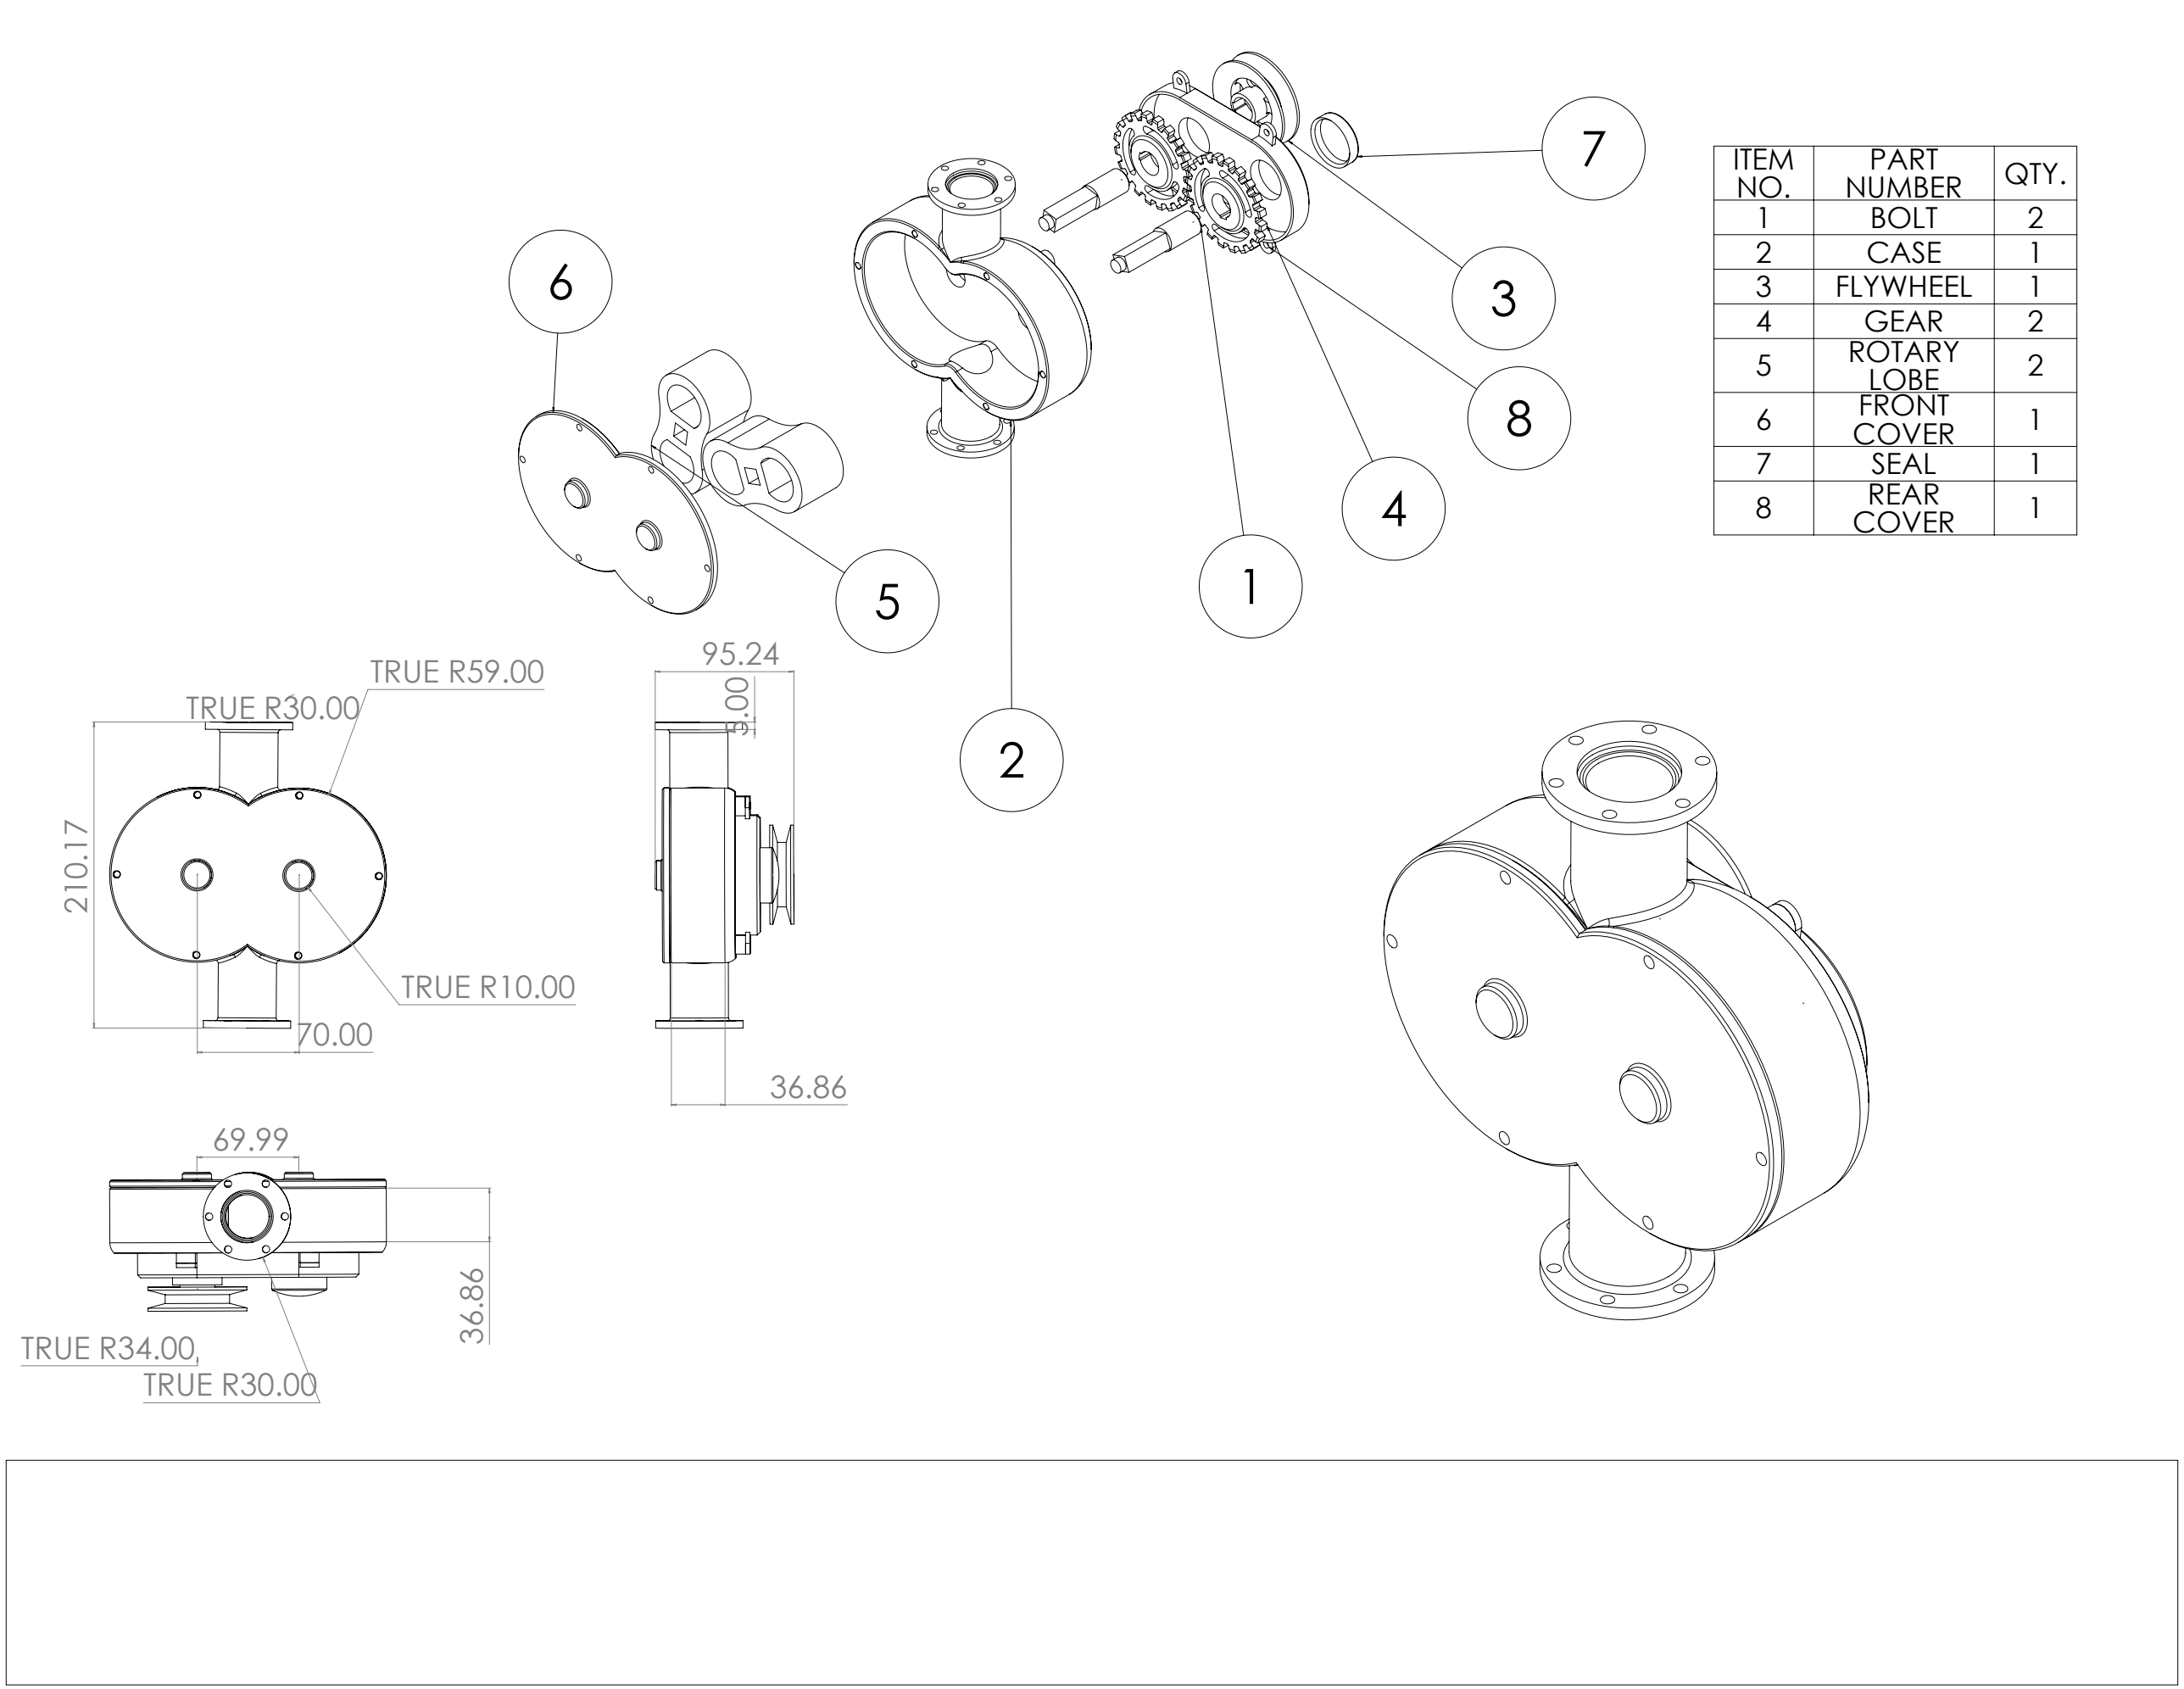
ISO-10303-21;
HEADER;
FILE_DESCRIPTION (('STEP AP214'),
    '1' );
FILE_NAME ('MAS-345',
    '2026-10-24T00:51:42',
    ( '' ),
    ( '' ),
    'SwSTEP 2.0',
    'SolidWorks 2025',
    '' );
FILE_SCHEMA (( 'AUTOMOTIVE_DESIGN' ));
ENDSEC;

DATA;
#1 = DIRECTION ( 'NONE',  ( 1.296372316667914327E-16, 1.000000000000000000, -0.000000000000000000 ) ) ;
#2 = DIRECTION ( 'NONE',  ( -1.000000000000000000, 0.000000000000000000, 0.000000000000000000 ) ) ;
#3 = EDGE_CURVE ( 'NONE', #16867, #19408, #6040, .T. ) ;
#4 = CIRCLE ( 'NONE', #2943, 3.000000000000002665 ) ;
#5 = ORIENTED_EDGE ( 'NONE', *, *, #17834, .T. ) ;
#6 = VECTOR ( 'NONE', #825, 1000.000000000000000 ) ;
#7 = VERTEX_POINT ( 'NONE', #19816 ) ;
#8 = LINE ( 'NONE', #12148, #20561 ) ;
#9 = CARTESIAN_POINT ( 'NONE',  ( 7.505578006075174891, 1.461761173328240959, -55.63523492904085543 ) ) ;
#10 = CYLINDRICAL_SURFACE ( 'NONE', #2581, 1.000000000000000888 ) ;
#11 = DIRECTION ( 'NONE',  ( -0.000000000000000000, 1.000000000000000000, -0.000000000000000000 ) ) ;
#12 = DIRECTION ( 'NONE',  ( -6.505213034913038160E-19, -3.903127820947822896E-18, -1.000000000000000000 ) ) ;
#13 = ORIENTED_EDGE ( 'NONE', *, *, #8232, .T. ) ;
#14 = LINE ( 'NONE', #10421, #6182 ) ;
#15 = CARTESIAN_POINT ( 'NONE',  ( -11.08851315719095609, 40.00000000000000000, -54.00022650832062254 ) ) ;
#16 = VERTEX_POINT ( 'NONE', #2397 ) ;
#17 = DIRECTION ( 'NONE',  ( 0.000000000000000000, -1.000000000000000000, 0.000000000000000000 ) ) ;
#18 = CARTESIAN_POINT ( 'NONE',  ( 17.25453130113929134, 34.47978402352274685, -57.33123263757907750 ) ) ;
#20 = CIRCLE ( 'NONE', #20518, 59.99999999999703704 ) ;
#19 = DIRECTION ( 'NONE',  ( -0.000000000000000000, -1.000000000000000000, -0.000000000000000000 ) ) ;
#21 = CARTESIAN_POINT ( 'NONE',  ( 7.552830766296163567, 40.00000000000000000, 52.78252194617787296 ) ) ;
#22 = CARTESIAN_POINT ( 'NONE',  ( 14.52224280010135615, 23.83254695043585869, -45.61498238574513664 ) ) ;
#23 = ORIENTED_EDGE ( 'NONE', *, *, #6487, .T. ) ;
#24 = DIRECTION ( 'NONE',  ( -6.505213034913038160E-19, -3.903127820947822896E-18, -1.000000000000000000 ) ) ;
#25 = CARTESIAN_POINT ( 'NONE',  ( -14.27302218980893578, 2.669631712211265828, 56.31136122552221934 ) ) ;
#26 = ADVANCED_FACE ( 'NONE', ( #12912 ), #4119, .F. ) ;
#27 = ORIENTED_EDGE ( 'NONE', *, *, #9694, .T. ) ;
#28 = DIRECTION ( 'NONE',  ( 0.000000000000000000, 1.000000000000000000, 0.000000000000000000 ) ) ;
#29 = CARTESIAN_POINT ( 'NONE',  ( -36.39375341857508062, -7.980461308160102796, -6.999999999999985789 ) ) ;
#30 = DIRECTION ( 'NONE',  ( -0.000000000000000000, -1.000000000000000000, -0.000000000000000000 ) ) ;
#31 = VERTEX_POINT ( 'NONE', #2518 ) ;
#32 = AXIS2_PLACEMENT_3D ( 'NONE', #9463, #19547, #3850 ) ;
#33 = ORIENTED_EDGE ( 'NONE', *, *, #2893, .T. ) ;
#34 = ORIENTED_EDGE ( 'NONE', *, *, #17370, .T. ) ;
#35 = ORIENTED_EDGE ( 'NONE', *, *, #15224, .F. ) ;
#36 = CARTESIAN_POINT ( 'NONE',  ( -2.396330562663482766, 23.84645203474120478, 6.679745199209158102 ) ) ;
#37 = CARTESIAN_POINT ( 'NONE',  ( 17.68664055422810932, 6.162676607241195370, 57.44855069909474565 ) ) ;
#38 = CARTESIAN_POINT ( 'NONE',  ( 9.260192184203184240, 40.00000000000000000, 53.42688922108487759 ) ) ;
#39 = EDGE_CURVE ( 'NONE', #4801, #16804, #900, .T. ) ;
#40 = ORIENTED_EDGE ( 'NONE', *, *, #1892, .T. ) ;
#41 = DIRECTION ( 'NONE',  ( 6.505213034913038160E-19, 3.903127820947822896E-18, 1.000000000000000000 ) ) ;
#42 = CARTESIAN_POINT ( 'NONE',  ( -0.5350771668691333138, 5.000000000000000888, 38.73397172404479960 ) ) ;
#43 = VERTEX_POINT ( 'NONE', #2740 ) ;
#44 = CARTESIAN_POINT ( 'NONE',  ( 4.012214033923966740E-15, -1.570715777137759117, 48.07784006879590066 ) ) ;
#45 = ORIENTED_EDGE ( 'NONE', *, *, #21489, .F. ) ;
#46 = CARTESIAN_POINT ( 'NONE',  ( -20.00000000000001421, 20.00000000000000000, -60.62177826491068799 ) ) ;
#47 = EDGE_LOOP ( 'NONE', ( #21691, #2135, #22378, #2493 ) ) ;
#48 = DIRECTION ( 'NONE',  ( -1.000000000000000000, -1.208970125616063644E-17, 0.000000000000000000 ) ) ;
#49 = ADVANCED_FACE ( 'NONE', ( #14857 ), #21880, .F. ) ;
#50 = CARTESIAN_POINT ( 'NONE',  ( 35.00000000000000000, -5.000000000000000888, -18.00000000000000000 ) ) ;
#51 = DIRECTION ( 'NONE',  ( 0.000000000000000000, 0.000000000000000000, -1.000000000000000000 ) ) ;
#52 = CARTESIAN_POINT ( 'NONE',  ( 19.96400288702118431, 18.50890182901837022, 60.61328093326561373 ) ) ;
#53 = DIRECTION ( 'NONE',  ( 0.000000000000000000, 0.000000000000000000, 1.000000000000000000 ) ) ;
#54 = CARTESIAN_POINT ( 'NONE',  ( -5.833333333333327708, 6.180730040185831164, 40.61164310337068173 ) ) ;
#55 = ORIENTED_EDGE ( 'NONE', *, *, #16648, .F. ) ;
#56 = AXIS2_PLACEMENT_3D ( 'NONE', #2091, #11020, #12611 ) ;
#57 = VERTEX_POINT ( 'NONE', #20717 ) ;
#58 = ORIENTED_EDGE ( 'NONE', *, *, #10603, .F. ) ;
#59 = ORIENTED_EDGE ( 'NONE', *, *, #871, .T. ) ;
#60 = DIRECTION ( 'NONE',  ( -0.000000000000000000, -0.000000000000000000, 1.000000000000000000 ) ) ;
#61 = CARTESIAN_POINT ( 'NONE',  ( -24.43377932785584505, 26.64693883069154623, -2.933296326616394278 ) ) ;
#62 = ADVANCED_FACE ( 'NONE', ( #18545 ), #20663, .F. ) ;
#63 = DIRECTION ( 'NONE',  ( -0.000000000000000000, -1.000000000000000000, -0.000000000000000000 ) ) ;
#64 = DIRECTION ( 'NONE',  ( 0.000000000000000000, 1.000000000000000000, 0.000000000000000000 ) ) ;
#65 = CARTESIAN_POINT ( 'NONE',  ( 2.244030701350347989, 39.96966515414118959, 50.39883264010746444 ) ) ;
#66 = VERTEX_POINT ( 'NONE', #2856 ) ;
#67 = DIRECTION ( 'NONE',  ( -0.000000000000000000, 1.000000000000000000, -0.000000000000000000 ) ) ;
#68 = CARTESIAN_POINT ( 'NONE',  ( -6.742883674876493316, -34.24928931925791176, -2.999999999999975131 ) ) ;
#69 = EDGE_CURVE ( 'NONE', #16039, #14303, #1275, .T. ) ;
#70 = CARTESIAN_POINT ( 'NONE',  ( -34.99999999999999289, 40.00000000000000000, 60.00000000000001421 ) ) ;
#71 = ADVANCED_FACE ( 'NONE', ( #20271 ), #22509, .T. ) ;
#72 = DIRECTION ( 'NONE',  ( -1.000000000000000000, 0.000000000000000000, 0.000000000000000000 ) ) ;
#73 = EDGE_CURVE ( 'NONE', #8231, #15027, #14429, .T. ) ;
#74 = VECTOR ( 'NONE', #6196, 1000.000000000000114 ) ;
#75 = CARTESIAN_POINT ( 'NONE',  ( -21.65063509461097269, 12.49999999999990052, -5.000000000000004441 ) ) ;
#76 = CARTESIAN_POINT ( 'NONE',  ( -8.123117863918686510, 39.63127865102772063, 53.85467328977310331 ) ) ;
#77 = DIRECTION ( 'NONE',  ( 0.000000000000000000, 0.000000000000000000, -1.000000000000000000 ) ) ;
#78 = CARTESIAN_POINT ( 'NONE',  ( 35.00000000000000000, 13.99999999999999822, 15.00000000000002132 ) ) ;
#79 = ADVANCED_FACE ( 'NONE', ( #15536 ), #15524, .T. ) ;
#80 = ORIENTED_EDGE ( 'NONE', *, *, #1374, .F. ) ;
#81 = ORIENTED_EDGE ( 'NONE', *, *, #16043, .F. ) ;
#82 = ORIENTED_EDGE ( 'NONE', *, *, #17683, .T. ) ;
#83 = CIRCLE ( 'NONE', #6686, 8.999999999999998224 ) ;
#84 = APPLICATION_CONTEXT ( 'automotive_design' ) ;
#85 = CIRCLE ( 'NONE', #13966, 31.50000000000000711 ) ;
#86 = DIRECTION ( 'NONE',  ( -0.000000000000000000, -1.000000000000000000, -0.000000000000000000 ) ) ;
#87 = DIRECTION ( 'NONE',  ( -1.000000000000000000, 0.000000000000000000, 0.000000000000000000 ) ) ;
#88 = DIRECTION ( 'NONE',  ( 0.000000000000000000, 0.000000000000000000, -1.000000000000000000 ) ) ;
#89 = DIRECTION ( 'NONE',  ( -0.000000000000000000, 1.000000000000000000, -0.000000000000000000 ) ) ;
#90 = CARTESIAN_POINT ( 'NONE',  ( -11.54473802384001324, 36.35512261685148871, -55.24115706042312013 ) ) ;
#91 = CARTESIAN_POINT ( 'NONE',  ( -14.50678847729824383, 23.83439465050324912, -45.60743157421818950 ) ) ;
#92 = EDGE_LOOP ( 'NONE', ( #21814, #17225, #4726, #11812 ) ) ;
#93 = DIRECTION ( 'NONE',  ( 1.445602896647339163E-16, -0.000000000000000000, 1.000000000000000000 ) ) ;
#94 = CARTESIAN_POINT ( 'NONE',  ( 2.775557561562891351E-14, -2.775557561562891351E-14, 2.999999999999999112 ) ) ;
#95 = DIRECTION ( 'NONE',  ( 0.7071067811865561215, 8.659560562355038861E-17, -0.7071067811865390240 ) ) ;
#96 = DIRECTION ( 'NONE',  ( -3.063596499322170048E-16, -0.000000000000000000, -1.000000000000000000 ) ) ;
#97 = EDGE_CURVE ( 'NONE', #13097, #7488, #538, .T. ) ;
#98 = ORIENTED_EDGE ( 'NONE', *, *, #9067, .T. ) ;
#99 = ADVANCED_FACE ( 'NONE', ( #13698 ), #18767, .T. ) ;
#100 = CARTESIAN_POINT ( 'NONE',  ( -22.28024240313497728, -22.26748298433262008, 3.000000000000023537 ) ) ;
#101 = CARTESIAN_POINT ( 'NONE',  ( 27.01645732367885699, 17.86915608785655252, -2.999999999999971578 ) ) ;
#102 = AXIS2_PLACEMENT_3D ( 'NONE', #16431, #14697, #2342 ) ;
#103 = EDGE_CURVE ( 'NONE', #20053, #16550, #22141, .T. ) ;
#104 = VERTEX_POINT ( 'NONE', #2968 ) ;
#105 = VERTEX_POINT ( 'NONE', #9938 ) ;
#106 = CARTESIAN_POINT ( 'NONE',  ( -1.568459684869329074, 24.67391323485165699, 8.880481854261958574 ) ) ;
#107 = CARTESIAN_POINT ( 'NONE',  ( 4.928914132345181612E-15, 5.025303850726727362, -19.00000000000000355 ) ) ;
#108 = CYLINDRICAL_SURFACE ( 'NONE', #5479, 2.500000000000002220 ) ;
#109 = AXIS2_PLACEMENT_3D ( 'NONE', #8322, #11535, #18749 ) ;
#110 = CARTESIAN_POINT ( 'NONE',  ( 90.00000000000000000, 40.00000000000000000, -2.099999999999991651 ) ) ;
#111 = B_SPLINE_CURVE_WITH_KNOTS ( 'NONE', 3,
 ( #17365, #18873, #3301, #3063 ),
 .UNSPECIFIED., .F., .F.,
 ( 4, 4 ),
 ( 0.001893031756885769868, 0.003808480026564024790 ),
 .UNSPECIFIED. ) ;
#112 = ORIENTED_EDGE ( 'NONE', *, *, #18556, .F. ) ;
#113 = DIRECTION ( 'NONE',  ( 0.000000000000000000, 0.000000000000000000, 1.000000000000000000 ) ) ;
#114 = CARTESIAN_POINT ( 'NONE',  ( -11.49398617737440986, 39.99999999999999289, 54.13866599136459001 ) ) ;
#115 = ORIENTED_EDGE ( 'NONE', *, *, #21368, .T. ) ;
#116 = DIRECTION ( 'NONE',  ( 6.505213034913038160E-19, 3.903127820947822896E-18, 1.000000000000000000 ) ) ;
#117 = CIRCLE ( 'NONE', #11814, 20.00000000000000000 ) ;
#118 = CARTESIAN_POINT ( 'NONE',  ( 14.34650594848453942, 37.25275621493270961, -56.33443587181653811 ) ) ;
#119 = DIRECTION ( 'NONE',  ( -6.505213034913038160E-19, -3.903127820947822896E-18, -1.000000000000000000 ) ) ;
#120 = CARTESIAN_POINT ( 'NONE',  ( 14.04383866228953259, 25.28361825225917769, -45.39674436955350245 ) ) ;
#121 = VERTEX_POINT ( 'NONE', #15312 ) ;
#122 = CARTESIAN_POINT ( 'NONE',  ( 4.000000000000007105, 28.19616000222403684, 4.898587196589412829E-16 ) ) ;
#123 = CARTESIAN_POINT ( 'NONE',  ( -1.321840103127373878, 39.98984252836526565, -49.73540240164955151 ) ) ;
#124 = ORIENTED_EDGE ( 'NONE', *, *, #15859, .T. ) ;
#125 = DIRECTION ( 'NONE',  ( -0.000000000000000000, -0.000000000000000000, 1.000000000000000000 ) ) ;
#126 = VECTOR ( 'NONE', #7524, 1000.000000000000000 ) ;
#127 = CARTESIAN_POINT ( 'NONE',  ( 4.177897941877304788, -34.13396246814587442, -2.999999999999999112 ) ) ;
#128 = CARTESIAN_POINT ( 'NONE',  ( -31.11077005834418685, 4.936596639065066405, 2.999999999999995559 ) ) ;
#129 = AXIS2_PLACEMENT_3D ( 'NONE', #9904, #8084, #22058 ) ;
#130 = AXIS2_PLACEMENT_3D ( 'NONE', #19374, #14408, #3677 ) ;
#131 = VERTEX_POINT ( 'NONE', #4797 ) ;
#132 = ORIENTED_EDGE ( 'NONE', *, *, #8958, .T. ) ;
#133 = ORIENTED_EDGE ( 'NONE', *, *, #15085, .T. ) ;
#134 = ADVANCED_FACE ( 'NONE', ( #4576 ), #8565, .F. ) ;
#135 = EDGE_LOOP ( 'NONE', ( #20964, #9442, #3465, #7281 ) ) ;
#136 = DIRECTION ( 'NONE',  ( 0.000000000000000000, 0.000000000000000000, -1.000000000000000000 ) ) ;
#137 = CARTESIAN_POINT ( 'NONE',  ( 42.50000000000000000, 10.00000000000000000, 47.49999999999999289 ) ) ;
#138 = DIRECTION ( 'NONE',  ( -0.000000000000000000, -1.000000000000000000, -0.000000000000000000 ) ) ;
#139 = CARTESIAN_POINT ( 'NONE',  ( 2.175117723777981293, 39.99999999999999289, 50.07592572012215015 ) ) ;
#140 = ORIENTED_EDGE ( 'NONE', *, *, #13576, .T. ) ;
#141 = FACE_BOUND ( 'NONE', #13024, .T. ) ;
#142 = DIRECTION ( 'NONE',  ( 0.000000000000000000, -0.000000000000000000, -1.000000000000000000 ) ) ;
#143 = ORIENTED_EDGE ( 'NONE', *, *, #2467, .F. ) ;
#144 = DIRECTION ( 'NONE',  ( 6.505213034913038160E-19, 3.903127820947822896E-18, 1.000000000000000000 ) ) ;
#145 = EDGE_CURVE ( 'NONE', #18194, #11720, #10158, .T. ) ;
#146 = VECTOR ( 'NONE', #10611, 1000.000000000000000 ) ;
#147 = CARTESIAN_POINT ( 'NONE',  ( 42.50000000000000000, 7.000000000000000000, 47.49999999999999289 ) ) ;
#148 = ORIENTED_EDGE ( 'NONE', *, *, #5497, .F. ) ;
#149 = CARTESIAN_POINT ( 'NONE',  ( -3.591923118226331086E-15, -4.883049072964007919, -45.13706194851761921 ) ) ;
#150 = ORIENTED_EDGE ( 'NONE', *, *, #14053, .T. ) ;
#151 = CARTESIAN_POINT ( 'NONE',  ( 8.331955809010642255, 38.18181818181816567, 56.36098470834075158 ) ) ;
#152 = DIRECTION ( 'NONE',  ( 1.000000000000000000, 0.000000000000000000, 0.000000000000000000 ) ) ;
#153 = CARTESIAN_POINT ( 'NONE',  ( -4.436826463219276206, 39.87775421764654027, 51.86208637039475633 ) ) ;
#154 = VECTOR ( 'NONE', #7572, 1000.000000000000114 ) ;
#155 = CARTESIAN_POINT ( 'NONE',  ( 16.16619463698827630, 31.79081685853978101, 57.00191113791574082 ) ) ;
#156 = PLANE ( 'NONE',  #2303 ) ;
#157 = DIRECTION ( 'NONE',  ( 0.000000000000000000, 0.000000000000000000, 1.000000000000000000 ) ) ;
#158 = CONICAL_SURFACE ( 'NONE', #22127, 2.524999999999999467, 0.7853981633973095011 ) ;
#159 = VERTEX_POINT ( 'NONE', #1574 ) ;
#160 = AXIS2_PLACEMENT_3D ( 'NONE', #15195, #16931, #6621 ) ;
#161 = ORIENTED_EDGE ( 'NONE', *, *, #622, .T. ) ;
#162 = ORIENTED_EDGE ( 'NONE', *, *, #20424, .T. ) ;
#163 = EDGE_CURVE ( 'NONE', #12184, #10164, #18107, .T. ) ;
#164 = VERTEX_POINT ( 'NONE', #8227 ) ;
#165 = CARTESIAN_POINT ( 'NONE',  ( -32.75570538720762670, 15.02862401740784293, -2.999999999999995559 ) ) ;
#166 = FACE_OUTER_BOUND ( 'NONE', #9561, .T. ) ;
#167 = CARTESIAN_POINT ( 'NONE',  ( 3.330669073875469621E-13, -1.110223024625156540E-13, -2.999999999999971578 ) ) ;
#168 = CARTESIAN_POINT ( 'NONE',  ( 0.9607529184257457278, 39.99453553102809877, 49.46704527242837912 ) ) ;
#169 = AXIS2_PLACEMENT_3D ( 'NONE', #17860, #14739, #16123 ) ;
#170 = B_SPLINE_CURVE_WITH_KNOTS ( 'NONE', 3,
 ( #22387, #25, #8397, #19283, #7015, #1634, #10434, #3588, #15593, #13972, #6677, #20996, #3128, #5083, #5301, #10546, #17549, #22616, #11941, #17094, #20771, #22497, #10215, #13635, #20652, #12275, #4959, #1859, #17430, #22274, #15253, #20548, #10099, #6572, #8504, #13532, #4852, #11822, #6912, #12059 ),
 .UNSPECIFIED., .F., .F.,
 ( 4, 2, 2, 2, 2, 2, 2, 2, 2, 2, 2, 2, 2, 2, 2, 2, 2, 2, 2, 4 ),
 ( 0.000000000000000000, 0.002766773850155583667, 0.004150160775233378320, 0.005533547700311173406, 0.008300321550466751436, 0.009683708475544540450, 0.01106709540062232947, 0.01660064310093350981, 0.01798403002601129883, 0.01936741695108909131, 0.02213419080124466934, 0.02490096465140025084, 0.02766773850155583581, 0.03043451235171141731, 0.03181789927678920632, 0.03320128620186699187, 0.03873483390217814792, 0.04011822082725592653, 0.04150160775233370514, 0.04426838160248924847 ),
 .UNSPECIFIED. ) ;
#171 = EDGE_CURVE ( 'NONE', #14638, #20199, #4931, .T. ) ;
#172 = ORIENTED_EDGE ( 'NONE', *, *, #12979, .T. ) ;
#173 = AXIS2_PLACEMENT_3D ( 'NONE', #16930, #17152, #13241 ) ;
#174 = CARTESIAN_POINT ( 'NONE',  ( 13.56354382738798847, 2.142135623730931471, -56.03997097393683191 ) ) ;
#175 = CARTESIAN_POINT ( 'NONE',  ( 2.220446049250313081E-13, 2.775557561562891351E-14, -2.800654218530485018 ) ) ;
#176 = DIRECTION ( 'NONE',  ( -0.5840452403773153112, 0.8117211080122311850, 0.000000000000000000 ) ) ;
#177 = LINE ( 'NONE', #21385, #3523 ) ;
#178 = CARTESIAN_POINT ( 'NONE',  ( 11.86180952233169705, 39.00000000000000000, 55.35904751184887118 ) ) ;
#179 = AXIS2_PLACEMENT_3D ( 'NONE', #12084, #11739, #22064 ) ;
#180 =( LENGTH_UNIT ( ) NAMED_UNIT ( * ) SI_UNIT ( .MILLI., .METRE. ) );
#181 = DIRECTION ( 'NONE',  ( 8.659560562354903276E-17, -0.7071067811865500152, 0.7071067811865451302 ) ) ;
#182 = EDGE_CURVE ( 'NONE', #4097, #21371, #18465, .T. ) ;
#183 = CARTESIAN_POINT ( 'NONE',  ( -42.49999999999996447, 7.000000000000000000, -47.50000000000000711 ) ) ;
#184 = CYLINDRICAL_SURFACE ( 'NONE', #1331, 6.499999999999999112 ) ;
#185 = AXIS2_PLACEMENT_3D ( 'NONE', #17657, #15929, #17553 ) ;
#186 = EDGE_LOOP ( 'NONE', ( #20186, #1645, #6973, #5901 ) ) ;
#187 = AXIS2_PLACEMENT_3D ( 'NONE', #2297, #17991, #16268 ) ;
#188 = ORIENTED_EDGE ( 'NONE', *, *, #1082, .F. ) ;
#189 = EDGE_CURVE ( 'NONE', #17751, #16070, #1466, .T. ) ;
#190 = EDGE_CURVE ( 'NONE', #16687, #2945, #6029, .T. ) ;
#191 = B_SPLINE_CURVE_WITH_KNOTS ( 'NONE', 3,
 ( #12236, #6868, #6982, #6529, #11779, #5041, #16942, #13938, #20733, #8239, #18781, #17166, #17055, #13836, #5157, #1362 ),
 .UNSPECIFIED., .F., .F.,
 ( 4, 2, 2, 2, 2, 2, 2, 4 ),
 ( 8.673617379884035472E-19, 0.003169695113379691204, 0.006339390226759381540, 0.007924237783449226274, 0.008716661561794153412, 0.009509085340139077080, 0.01109393289682892789, 0.01267878045351877869 ),
 .UNSPECIFIED. ) ;
#192 = EDGE_LOOP ( 'NONE', ( #22045, #625, #16460, #5308 ) ) ;
#193 = CARTESIAN_POINT ( 'NONE',  ( 9.367793990832831597, -4.928932186891253231, -51.00106331756588673 ) ) ;
#194 = CARTESIAN_POINT ( 'NONE',  ( 11.45074849662552197, 39.99999999999999289, -54.12667998692793958 ) ) ;
#195 = DIRECTION ( 'NONE',  ( 6.505213034913038160E-19, 3.903127820947822896E-18, 1.000000000000000000 ) ) ;
#196 = EDGE_CURVE ( 'NONE', #9340, #20230, #6736, .T. ) ;
#197 = LINE ( 'NONE', #10969, #5945 ) ;
#198 = DIRECTION ( 'NONE',  ( -0.1421319796954322312, 0.000000000000000000, -0.9898477157360405787 ) ) ;
#199 = VECTOR ( 'NONE', #3023, 1000.000000000000000 ) ;
#200 = CARTESIAN_POINT ( 'NONE',  ( -15.91103418227302058, 35.86133518681679533, -56.88632568426858427 ) ) ;
#201 = AXIS2_PLACEMENT_3D ( 'NONE', #4772, #15280, #6939 ) ;
#202 = CARTESIAN_POINT ( 'NONE',  ( -35.00000000000000000, 14.00000000000000000, 39.00000000000002132 ) ) ;
#203 = AXIS2_PLACEMENT_3D ( 'NONE', #6824, #20803, #5115 ) ;
#204 = ORIENTED_EDGE ( 'NONE', *, *, #20103, .T. ) ;
#205 = CYLINDRICAL_SURFACE ( 'NONE', #8297, 59.99999999999700862 ) ;
#206 = CARTESIAN_POINT ( 'NONE',  ( -11.35354668330701422, -30.33632613426187774, 2.999999999999999112 ) ) ;
#207 = DIRECTION ( 'NONE',  ( 1.000000000000000000, 0.000000000000000000, 1.224646799147352961E-16 ) ) ;
#208 = ADVANCED_FACE ( 'NONE', ( #17833 ), #17377, .F. ) ;
#209 = CARTESIAN_POINT ( 'NONE',  ( -26.64365646977275048, -17.09029715894938661, -6.999999999999950262 ) ) ;
#210 = CARTESIAN_POINT ( 'NONE',  ( 35.00000000000001421, 5.000000000000000000, 1.540743955509788682E-30 ) ) ;
#211 = CIRCLE ( 'NONE', #1322, 34.90673715956759082 ) ;
#212 = EDGE_LOOP ( 'NONE', ( #4099, #12246, #12145, #6281 ) ) ;
#213 = EDGE_CURVE ( 'NONE', #13383, #4605, #12223, .T. ) ;
#214 = DIRECTION ( 'NONE',  ( 6.505213034913038160E-19, 3.903127820947822896E-18, 1.000000000000000000 ) ) ;
#215 = DIRECTION ( 'NONE',  ( 0.000000000000000000, 1.000000000000000000, 0.000000000000000000 ) ) ;
#216 = VECTOR ( 'NONE', #1494, 1000.000000000000114 ) ;
#217 = AXIS2_PLACEMENT_3D ( 'NONE', #4678, #12107, #11654 ) ;
#218 = EDGE_CURVE ( 'NONE', #13519, #1842, #5991, .T. ) ;
#219 = ORIENTED_EDGE ( 'NONE', *, *, #7330, .T. ) ;
#220 = AXIS2_PLACEMENT_3D ( 'NONE', #14083, #12166, #15923 ) ;
#221 = AXIS2_PLACEMENT_3D ( 'NONE', #15560, #3559, #10737 ) ;
#222 = ITEM_DEFINED_TRANSFORMATION ( 'NONE', 'NONE', #3273,  #18273 ) ;
#223 = ADVANCED_FACE ( 'NONE', ( #21279 ), #5571, .F. ) ;
#224 = ORIENTED_EDGE ( 'NONE', *, *, #266, .F. ) ;
#225 = CARTESIAN_POINT ( 'NONE',  ( 35.00000000000001421, 5.000000000000000000, 1.540743955509788682E-30 ) ) ;
#226 = CARTESIAN_POINT ( 'NONE',  ( -1.387778780781445676E-14, 20.00000000000000000, -105.0020000000000095 ) ) ;
#227 = CARTESIAN_POINT ( 'NONE',  ( -34.99999999999999289, 0.000000000000000000, -3.012171160963566127E-14 ) ) ;
#228 = CARTESIAN_POINT ( 'NONE',  ( 11.93772187171674126, 33.46652738560661788, -3.000000000000018208 ) ) ;
#229 = ORIENTED_EDGE ( 'NONE', *, *, #280, .F. ) ;
#230 = DIRECTION ( 'NONE',  ( 1.000000000000000000, 0.000000000000000000, 0.000000000000000000 ) ) ;
#231 = CARTESIAN_POINT ( 'NONE',  ( -9.062586715439731933, 2.130694986425758941, -54.31128890270724696 ) ) ;
#232 = ORIENTED_EDGE ( 'NONE', *, *, #1295, .T. ) ;
#233 = DIRECTION ( 'NONE',  ( 0.000000000000000000, -1.000000000000000000, 0.000000000000000000 ) ) ;
#234 = CARTESIAN_POINT ( 'NONE',  ( 17.14099744770036082, 5.493236686326223861, -57.28126710884282602 ) ) ;
#235 = CARTESIAN_POINT ( 'NONE',  ( 34.00000000000000000, -8.251288694035739724, 4.163799117101000559E-15 ) ) ;
#236 = FACE_OUTER_BOUND ( 'NONE', #19875, .T. ) ;
#237 = ORIENTED_EDGE ( 'NONE', *, *, #15109, .F. ) ;
#238 = DIRECTION ( 'NONE',  ( -1.000000000000000000, 0.000000000000000000, 0.000000000000000000 ) ) ;
#239 = FACE_OUTER_BOUND ( 'NONE', #8251, .T. ) ;
#240 = CARTESIAN_POINT ( 'NONE',  ( -7.031141255823502689, 39.67715640622406426, -53.36152254753006474 ) ) ;
#241 = AXIS2_PLACEMENT_3D ( 'NONE', #20174, #2191, #19945 ) ;
#242 = EDGE_LOOP ( 'NONE', ( #11934, #16526 ) ) ;
#243 = LINE ( 'NONE', #20894, #20346 ) ;
#244 = CARTESIAN_POINT ( 'NONE',  ( -2.496587642955530040, 0.1153990516131219446, 52.32802461649446002 ) ) ;
#245 = VECTOR ( 'NONE', #16073, 1000.000000000000000 ) ;
#246 = ORIENTED_EDGE ( 'NONE', *, *, #18367, .T. ) ;
#247 = ORIENTED_EDGE ( 'NONE', *, *, #15444, .T. ) ;
#248 = AXIS2_PLACEMENT_3D ( 'NONE', #3692, #16267, #11111 ) ;
#249 = VERTEX_POINT ( 'NONE', #19225 ) ;
#250 =( NAMED_UNIT ( * ) SI_UNIT ( $, .STERADIAN. ) SOLID_ANGLE_UNIT ( ) );
#251 = EDGE_CURVE ( 'NONE', #17561, #8959, #16232, .T. ) ;
#252 = ORIENTED_EDGE ( 'NONE', *, *, #20268, .F. ) ;
#253 = LINE ( 'NONE', #3817, #4827 ) ;
#254 = DIRECTION ( 'NONE',  ( -0.000000000000000000, -0.000000000000000000, -1.000000000000000000 ) ) ;
#255 = CARTESIAN_POINT ( 'NONE',  ( 35.00000000000000000, 17.00000000000000000, -40.99999999999997868 ) ) ;
#256 = CARTESIAN_POINT ( 'NONE',  ( 7.563456360162507330, 39.99999999999999289, 52.78701495172266078 ) ) ;
#257 = ORIENTED_EDGE ( 'NONE', *, *, #16349, .T. ) ;
#258 = DIRECTION ( 'NONE',  ( -1.000000000000000000, -1.208970125616081209E-17, 0.000000000000000000 ) ) ;
#259 = FACE_BOUND ( 'NONE', #21033, .T. ) ;
#260 = VERTEX_POINT ( 'NONE', #22683 ) ;
#261 = CARTESIAN_POINT ( 'NONE',  ( -2.999999999999999112, 30.00000000000000000, 8.485281374238567764 ) ) ;
#262 = CARTESIAN_POINT ( 'NONE',  ( 7.325260514639500961E-15, -4.648749848371387827, 45.43309249825157536 ) ) ;
#263 = DIRECTION ( 'NONE',  ( 1.000000000000000000, 0.000000000000000000, 0.000000000000000000 ) ) ;
#264 = EDGE_LOOP ( 'NONE', ( #1620, #15292, #18249, #3062 ) ) ;
#265 = CYLINDRICAL_SURFACE ( 'NONE', #18235, 10.00000000000000000 ) ;
#266 = EDGE_CURVE ( 'NONE', #2332, #7531, #8895, .T. ) ;
#267 = EDGE_LOOP ( 'NONE', ( #12609, #14006, #18826, #6601, #2906, #9922, #5735, #20678 ) ) ;
#268 = CARTESIAN_POINT ( 'NONE',  ( -34.99999999999980815, 40.00000000000000711, 52.47499999999922693 ) ) ;
#269 = CARTESIAN_POINT ( 'NONE',  ( -0.3104238174410937634, 39.99820335227858692, 49.10409449009599570 ) ) ;
#270 = CARTESIAN_POINT ( 'NONE',  ( -35.00000000000000000, 40.00000000000000000, 1.387778780781445676E-14 ) ) ;
#271 = CARTESIAN_POINT ( 'NONE',  ( -12.00937115242646591, -34.74700806321101254, 2.800654218530512551 ) ) ;
#272 = VECTOR ( 'NONE', #9542, 1000.000000000000000 ) ;
#273 = VECTOR ( 'NONE', #6613, 1000.000000000000000 ) ;
#274 = CARTESIAN_POINT ( 'NONE',  ( 21.98712579307491666, 15.48449832074051358, 58.57208548029188222 ) ) ;
#275 = CARTESIAN_POINT ( 'NONE',  ( 17.79229176513301525, 31.47226199422865278, -2.933296326616372074 ) ) ;
#276 = AXIS2_PLACEMENT_3D ( 'NONE', #12018, #17271, #16939 ) ;
#277 = ADVANCED_FACE ( 'NONE', ( #12548, #8677, #5469, #19561, #10835, #1813, #15871, #8796, #9131 ), #15657, .T. ) ;
#278 = CARTESIAN_POINT ( 'NONE',  ( -25.58633464742629471, -23.74488952252781715, -2.999999999999975131 ) ) ;
#279 = ORIENTED_EDGE ( 'NONE', *, *, #15136, .F. ) ;
#280 = EDGE_CURVE ( 'NONE', #4403, #3845, #2016, .T. ) ;
#281 = ORIENTED_EDGE ( 'NONE', *, *, #17376, .F. ) ;
#282 = AXIS2_PLACEMENT_3D ( 'NONE', #21094, #12372, #5501 ) ;
#283 = ORIENTED_EDGE ( 'NONE', *, *, #5855, .F. ) ;
#284 = EDGE_LOOP ( 'NONE', ( #20837, #17843 ) ) ;
#285 = CARTESIAN_POINT ( 'NONE',  ( -9.689843208404443686, 39.33333333333332860, 54.54983754392751649 ) ) ;
#286 = DIRECTION ( 'NONE',  ( 1.000000000000000000, -1.084202172485504927E-16, 0.000000000000000000 ) ) ;
#287 = AXIS2_PLACEMENT_3D ( 'NONE', #18901, #20854, #8577 ) ;
#288 = DIRECTION ( 'NONE',  ( 0.000000000000000000, 0.000000000000000000, -1.000000000000000000 ) ) ;
#289 = VECTOR ( 'NONE', #14140, 1000.000000000000000 ) ;
#290 = DIRECTION ( 'NONE',  ( 1.000000000000000000, 0.000000000000000000, 0.000000000000000000 ) ) ;
#291 = B_SPLINE_CURVE_WITH_KNOTS ( 'NONE', 3,
 ( #8113, #6044, #21633, #5929, #14842, #9709 ),
 .UNSPECIFIED., .F., .F.,
 ( 4, 2, 4 ),
 ( 1.788112030672749005E-18, 0.002694896630591163932, 0.005389793261182326128 ),
 .UNSPECIFIED. ) ;
#292 = DIRECTION ( 'NONE',  ( 0.000000000000000000, -1.000000000000000000, 0.000000000000000000 ) ) ;
#293 = CARTESIAN_POINT ( 'NONE',  ( 3.944370656192286440, 39.90454853199823759, 51.54919367184183443 ) ) ;
#294 = CIRCLE ( 'NONE', #3228, 34.90673715956759082 ) ;
#295 = VERTEX_POINT ( 'NONE', #13926 ) ;
#296 = DIRECTION ( 'NONE',  ( 0.000000000000000000, 0.000000000000000000, -1.000000000000000000 ) ) ;
#297 = CARTESIAN_POINT ( 'NONE',  ( -42.50000000000000711, -12.00000000000000000, -47.50000000000000000 ) ) ;
#298 = DIRECTION ( 'NONE',  ( -1.000000000000000000, 0.000000000000000000, 0.000000000000000000 ) ) ;
#299 = FACE_OUTER_BOUND ( 'NONE', #1043, .T. ) ;
#300 = CARTESIAN_POINT ( 'NONE',  ( -34.99999999999999289, -5.000000000000000000, -54.99999999999705125 ) ) ;
#301 = AXIS2_PLACEMENT_3D ( 'NONE', #19951, #21671, #11581 ) ;
#302 = FACE_OUTER_BOUND ( 'NONE', #6391, .T. ) ;
#303 = EDGE_CURVE ( 'NONE', #11367, #19446, #9654, .T. ) ;
#304 = VECTOR ( 'NONE', #3939, 1000.000000000000000 ) ;
#305 = AXIS2_PLACEMENT_3D ( 'NONE', #12969, #11033, #9203 ) ;
#306 = PRODUCT_DEFINITION ( 'UNKNOWN', '', #18641, #21271 ) ;
#307 = DIRECTION ( 'NONE',  ( 1.000000000000000000, 0.000000000000000000, 0.000000000000000000 ) ) ;
#308 = DIRECTION ( 'NONE',  ( 0.000000000000000000, -1.000000000000000000, 0.000000000000000000 ) ) ;
#309 = AXIS2_PLACEMENT_3D ( 'NONE', #21426, #5731, #12703 ) ;
#310 = ORIENTED_EDGE ( 'NONE', *, *, #5485, .T. ) ;
#311 = ADVANCED_FACE ( 'NONE', ( #9013 ), #19696, .F. ) ;
#312 = VERTEX_POINT ( 'NONE', #7642 ) ;
#313 = ORIENTED_EDGE ( 'NONE', *, *, #10353, .F. ) ;
#314 = CARTESIAN_POINT ( 'NONE',  ( -2.999999999999999112, 22.00000000000000355, 8.485281374238567764 ) ) ;
#315 = AXIS2_PLACEMENT_3D ( 'NONE', #10190, #17183, #1262 ) ;
#316 = AXIS2_PLACEMENT_3D ( 'NONE', #15240, #12961, #19969 ) ;
#317 = FACE_OUTER_BOUND ( 'NONE', #17252, .T. ) ;
#318 = CARTESIAN_POINT ( 'NONE',  ( -26.50842683089743446, 24.41514043009193458, -2.999999999999975131 ) ) ;
#319 = DIRECTION ( 'NONE',  ( -0.000000000000000000, 1.000000000000000000, -0.000000000000000000 ) ) ;
#320 = EDGE_CURVE ( 'NONE', #13797, #13818, #18394, .T. ) ;
#321 = LINE ( 'NONE', #15778, #8511 ) ;
#322 = CARTESIAN_POINT ( 'NONE',  ( -20.00000000000001421, 19.20373330966867798, 60.62177826491072352 ) ) ;
#323 = CARTESIAN_POINT ( 'NONE',  ( 4.683984772515712893E-15, 6.000000000000019540, -17.00000000000000355 ) ) ;
#324 = PRODUCT_DEFINITION_FORMATION_WITH_SPECIFIED_SOURCE ( 'ANY', '', #1799, .NOT_KNOWN. ) ;
#325 = CARTESIAN_POINT ( 'NONE',  ( -15.00000000000001421, 20.00000000000000000, -45.82575694955838230 ) ) ;
#326 = EDGE_LOOP ( 'NONE', ( #11952, #8295, #15497, #872 ) ) ;
#327 = CARTESIAN_POINT ( 'NONE',  ( 5.551115123125782702E-14, -1.387778780781445676E-13, -5.749999999999949374 ) ) ;
#328 = CARTESIAN_POINT ( 'NONE',  ( -35.00000000000000000, 17.00000000000000000, 2.365113165210053967E-14 ) ) ;
#329 = CARTESIAN_POINT ( 'NONE',  ( -1.387778780781445676E-14, 20.00000000000000000, 98.00000000000000000 ) ) ;
#330 = DIRECTION ( 'NONE',  ( 0.000000000000000000, 0.000000000000000000, -1.000000000000000000 ) ) ;
#331 = EDGE_CURVE ( 'NONE', #8378, #6859, #4945, .T. ) ;
#332 = DIRECTION ( 'NONE',  ( 6.505213034913038160E-19, 3.903127820947822896E-18, 1.000000000000000000 ) ) ;
#333 = ORIENTED_EDGE ( 'NONE', *, *, #2752, .T. ) ;
#334 = FACE_OUTER_BOUND ( 'NONE', #3737, .T. ) ;
#335 = DIRECTION ( 'NONE',  ( 6.505213034913038160E-19, 3.903127820947822896E-18, 1.000000000000000000 ) ) ;
#336 = VECTOR ( 'NONE', #1062, 1000.000000000000000 ) ;
#337 = DIRECTION ( 'NONE',  ( 0.000000000000000000, -1.000000000000000000, 0.000000000000000000 ) ) ;
#338 = ORIENTED_EDGE ( 'NONE', *, *, #3032, .F. ) ;
#339 =( BOUNDED_SURFACE ( )  B_SPLINE_SURFACE ( 3, 2, ( 
 ( #20618, #22011, #20293 ),
 ( #20513, #13386, #1148 ),
 ( #11788, #8141, #20176 ),
 ( #4597, #4928, #11578 ),
 ( #1371, #10065, #17063 ),
 ( #3217, #18567, #8367 ) ),
 .UNSPECIFIED., .F., .F., .F. ) 
 B_SPLINE_SURFACE_WITH_KNOTS ( ( 4, 2, 4 ),
 ( 3, 3 ),
 ( 0.000000000000000000, 0.002858401832365834675, 0.005716803664731669350 ),
 ( 0.000000000000000000, 1.000000000000000000 ),
 .UNSPECIFIED. ) 
 GEOMETRIC_REPRESENTATION_ITEM ( )  RATIONAL_B_SPLINE_SURFACE ( (
 ( 1.000000000000000000, 0.7200096751079140267, 1.000000000000000000),
 ( 1.000000000000000000, 0.7065285139735018038, 1.000000000000000000),
 ( 1.000000000000000000, 0.6920701671002518207, 1.000000000000000000),
 ( 1.000000000000000000, 0.6615687397045608709, 1.000000000000000000),
 ( 1.000000000000000000, 0.6455195629511447653, 1.000000000000000000),
 ( 1.000000000000000000, 0.6290213284793418902, 1.000000000000000000) ) ) 
 REPRESENTATION_ITEM ( '' )  SURFACE ( )  );
#340 = ORIENTED_EDGE ( 'NONE', *, *, #16660, .T. ) ;
#341 = CARTESIAN_POINT ( 'NONE',  ( 0.2660997432313502165, 39.99958209296121225, -48.93999222993210196 ) ) ;
#342 = DIRECTION ( 'NONE',  ( -1.000000000000000000, 0.000000000000000000, 0.000000000000000000 ) ) ;
#343 = CARTESIAN_POINT ( 'NONE',  ( -11.68090480754633553, 3.765577839755389622, 57.90797000640144176 ) ) ;
#344 = ADVANCED_FACE ( 'NONE', ( #7407, #531 ), #16341, .T. ) ;
#345 = DIRECTION ( 'NONE',  ( 6.505213034913038160E-19, 3.903127820947822896E-18, 1.000000000000000000 ) ) ;
#346 = ORIENTED_EDGE ( 'NONE', *, *, #17247, .F. ) ;
#347 = DIRECTION ( 'NONE',  ( 0.000000000000000000, 1.000000000000000000, 0.000000000000000000 ) ) ;
#348 = CARTESIAN_POINT ( 'NONE',  ( -6.444993702122386203, 40.00000000000000711, 52.30045897829974422 ) ) ;
#349 = VERTEX_POINT ( 'NONE', #14379 ) ;
#350 = DIRECTION ( 'NONE',  ( 0.000000000000000000, 0.000000000000000000, -1.000000000000000000 ) ) ;
#351 = CARTESIAN_POINT ( 'NONE',  ( 18.51338123223699483, 7.266791589766445014, -57.69263490290608587 ) ) ;
#352 = DIRECTION ( 'NONE',  ( 1.000000000000000000, 0.000000000000000000, 0.000000000000000000 ) ) ;
#353 = VERTEX_POINT ( 'NONE', #21620 ) ;
#354 = DIRECTION ( 'NONE',  ( 1.296372316667914327E-16, 1.000000000000000000, -0.000000000000000000 ) ) ;
#355 = DIRECTION ( 'NONE',  ( -0.000000000000000000, 1.000000000000000000, -0.000000000000000000 ) ) ;
#356 = EDGE_CURVE ( 'NONE', #18097, #20626, #19791, .T. ) ;
#357 = EDGE_CURVE ( 'NONE', #922, #13123, #3450, .T. ) ;
#358 = CARTESIAN_POINT ( 'NONE',  ( -0.4769535673226554806, 39.99865963977220673, -49.10163031951724122 ) ) ;
#359 = EDGE_CURVE ( 'NONE', #22631, #14416, #10776, .T. ) ;
#360 = ORIENTED_EDGE ( 'NONE', *, *, #18003, .F. ) ;
#361 = DIRECTION ( 'NONE',  ( -1.000000000000000000, -1.208970125616060717E-17, 0.000000000000000000 ) ) ;
#362 = CARTESIAN_POINT ( 'NONE',  ( 35.00000000000000000, 0.000000000000000000, 2.365113165210053967E-14 ) ) ;
#363 = CIRCLE ( 'NONE', #12085, 1.000000000000000888 ) ;
#364 = EDGE_CURVE ( 'NONE', #16, #13103, #12663, .T. ) ;
#365 = ORIENTED_EDGE ( 'NONE', *, *, #6652, .F. ) ;
#366 = B_SPLINE_CURVE_WITH_KNOTS ( 'NONE', 3,
 ( #12902, #16119, #9147, #665 ),
 .UNSPECIFIED., .F., .F.,
 ( 4, 4 ),
 ( 0.001893031756885595529, 0.003808480026563915502 ),
 .UNSPECIFIED. ) ;
#367 = EDGE_LOOP ( 'NONE', ( #19878, #14451, #14553, #14113 ) ) ;
#368 = EDGE_LOOP ( 'NONE', ( #6095, #15311 ) ) ;
#369 = B_SPLINE_CURVE_WITH_KNOTS ( 'NONE', 3,
 ( #18817, #9981, #13409, #16973, #17087, #15470 ),
 .UNSPECIFIED., .F., .F.,
 ( 4, 2, 4 ),
 ( 1.978164943978792966E-18, 0.005389490931282729137, 0.01077898186256545654 ),
 .UNSPECIFIED. ) ;
#370 = ORIENTED_EDGE ( 'NONE', *, *, #8346, .T. ) ;
#371 = CARTESIAN_POINT ( 'NONE',  ( -34.99999999999980815, 39.97500000000000142, 52.49999999999922551 ) ) ;
#372 = AXIS2_PLACEMENT_3D ( 'NONE', #19827, #18095, #3326 ) ;
#373 = DIRECTION ( 'NONE',  ( -0.000000000000000000, 1.000000000000000000, -0.000000000000000000 ) ) ;
#374 = CARTESIAN_POINT ( 'NONE',  ( 0.3946982817249323205, 39.99999999999999289, 48.99018268902280226 ) ) ;
#375 = ORIENTED_EDGE ( 'NONE', *, *, #11869, .T. ) ;
#376 = DIRECTION ( 'NONE',  ( 1.000000000000000000, 0.000000000000000000, 0.000000000000000000 ) ) ;
#377 = DIRECTION ( 'NONE',  ( 6.505213034913038160E-19, 3.903127820947822896E-18, 1.000000000000000000 ) ) ;
#378 = ORIENTED_EDGE ( 'NONE', *, *, #15742, .T. ) ;
#379 = CARTESIAN_POINT ( 'NONE',  ( -13.85640646055084702, -1.500000000000011768, 7.999999999999705125 ) ) ;
#380 = CARTESIAN_POINT ( 'NONE',  ( -21.21578383525638145, 27.34973130705545685, -58.39578210113618439 ) ) ;
#381 = CARTESIAN_POINT ( 'NONE',  ( 21.69517388068236841, 28.13960001536964128, -3.000000000000001776 ) ) ;
#382 = DIRECTION ( 'NONE',  ( -6.505213034913038160E-19, -3.903127820947822896E-18, -1.000000000000000000 ) ) ;
#383 = CARTESIAN_POINT ( 'NONE',  ( 0.3709469612214016387, -0.009390992346610399152, 50.78654667931946420 ) ) ;
#384 = VERTEX_POINT ( 'NONE', #9359 ) ;
#385 = CARTESIAN_POINT ( 'NONE',  ( 3.981168190751217750, 39.90684668434315086, -51.58237481356633225 ) ) ;
#386 = CARTESIAN_POINT ( 'NONE',  ( -3.210361346424068341, 39.75306810546534564, 52.30715206667691319 ) ) ;
#387 = CARTESIAN_POINT ( 'NONE',  ( 5.007713804312083461, 0.5950132857128228592, 54.03314628406707243 ) ) ;
#388 = ORIENTED_EDGE ( 'NONE', *, *, #9153, .F. ) ;
#389 = CARTESIAN_POINT ( 'NONE',  ( 21.77460018174823020, 14.53841458819210786, 58.52494103856225394 ) ) ;
#390 = DIRECTION ( 'NONE',  ( -0.000000000000000000, 1.000000000000000000, -0.000000000000000000 ) ) ;
#391 = ADVANCED_FACE ( 'NONE', ( #12888 ), #6369, .F. ) ;
#392 = AXIS2_PLACEMENT_3D ( 'NONE', #21456, #373, #16290 ) ;
#393 = ADVANCED_FACE ( 'NONE', ( #19897 ), #22473, .F. ) ;
#394 = FACE_BOUND ( 'NONE', #4049, .T. ) ;
#395 = EDGE_LOOP ( 'NONE', ( #16035, #6473, #11617, #1674 ) ) ;
#396 = ORIENTED_EDGE ( 'NONE', *, *, #11487, .T. ) ;
#397 = EDGE_CURVE ( 'NONE', #22398, #3259, #6731, .T. ) ;
#398 = EDGE_LOOP ( 'NONE', ( #11515, #3826 ) ) ;
#399 = ORIENTED_EDGE ( 'NONE', *, *, #73, .F. ) ;
#400 = DIRECTION ( 'NONE',  ( 0.000000000000000000, 0.000000000000000000, -1.000000000000000000 ) ) ;
#401 = CARTESIAN_POINT ( 'NONE',  ( 5.999999999999999112, -40.00000000000000000, -6.000000000000000000 ) ) ;
#402 = CARTESIAN_POINT ( 'NONE',  ( -35.79662727779878395, 4.171001175319294596, 3.000000000000006217 ) ) ;
#403 = ORIENTED_EDGE ( 'NONE', *, *, #16215, .T. ) ;
#404 = CARTESIAN_POINT ( 'NONE',  ( 8.215393105052410050, 1.749144060401382594, 56.08634520685871649 ) ) ;
#405 = CARTESIAN_POINT ( 'NONE',  ( -41.39271818392636959, 10.00000000000000000, -5.943569790512535533 ) ) ;
#406 = VECTOR ( 'NONE', #10198, 1000.000000000000000 ) ;
#407 = VERTEX_POINT ( 'NONE', #7982 ) ;
#408 = CARTESIAN_POINT ( 'NONE',  ( 90.00000000000000000, 40.00000000000000000, -9.108981535246192915E-16 ) ) ;
#409 = PRODUCT_DEFINITION_CONTEXT ( 'detailed design', #19716, 'design' ) ;
#410 = LINE ( 'NONE', #7295, #19704 ) ;
#411 = CARTESIAN_POINT ( 'NONE',  ( 2.775557561562891351E-14, 2.775557561562891351E-14, 5.750000000000001776 ) ) ;
#412 = LINE ( 'NONE', #12881, #16434 ) ;
#413 = DIRECTION ( 'NONE',  ( -0.000000000000000000, 1.000000000000000000, -0.000000000000000000 ) ) ;
#414 = CIRCLE ( 'NONE', #13204, 4.000000000000000000 ) ;
#415 = DIRECTION ( 'NONE',  ( 1.000000000000000000, 0.000000000000000000, 0.000000000000000000 ) ) ;
#416 = CYLINDRICAL_SURFACE ( 'NONE', #20007, 2.500000000000002220 ) ;
#417 = B_SPLINE_CURVE_WITH_KNOTS ( 'NONE', 3,
 ( #9345, #17934, #21264, #14708 ),
 .UNSPECIFIED., .F., .F.,
 ( 4, 4 ),
 ( 9.545285770746368752E-07, 0.001900595205834774504 ),
 .UNSPECIFIED. ) ;
#418 = ORIENTED_EDGE ( 'NONE', *, *, #9253, .T. ) ;
#419 = ORIENTED_EDGE ( 'NONE', *, *, #14863, .F. ) ;
#420 = ORIENTED_EDGE ( 'NONE', *, *, #17534, .T. ) ;
#421 = PLANE ( 'NONE',  #17700 ) ;
#422 = CARTESIAN_POINT ( 'NONE',  ( 34.00000000000000000, 8.251288694035739724, 4.163799117100999770E-15 ) ) ;
#423 = EDGE_CURVE ( 'NONE', #6835, #14085, #18431, .T. ) ;
#424 = DIRECTION ( 'NONE',  ( 0.000000000000000000, -1.000000000000000000, 0.000000000000000000 ) ) ;
#425 = CARTESIAN_POINT ( 'NONE',  ( -15.99999999999994493, 20.00000000000000355, 102.0000000000000142 ) ) ;
#426 = DIRECTION ( 'NONE',  ( -3.063596499322173499E-16, 0.000000000000000000, 1.000000000000000000 ) ) ;
#427 = LINE ( 'NONE', #14393, #10875 ) ;
#428 = DIRECTION ( 'NONE',  ( 0.000000000000000000, 0.000000000000000000, -1.000000000000000000 ) ) ;
#429 = FACE_OUTER_BOUND ( 'NONE', #19761, .T. ) ;
#430 = ADVANCED_FACE ( 'NONE', ( #15166 ), #13332, .T. ) ;
#431 = EDGE_CURVE ( 'NONE', #18746, #22096, #8909, .T. ) ;
#432 = ORIENTED_EDGE ( 'NONE', *, *, #17613, .T. ) ;
#433 = CARTESIAN_POINT ( 'NONE',  ( -1.387778780781445518E-14, 20.00000000000000355, 105.0000000000000142 ) ) ;
#434 = CARTESIAN_POINT ( 'NONE',  ( -4.240553750831113966, 39.54840718952534218, -53.29860200223215827 ) ) ;
#435 = DIRECTION ( 'NONE',  ( -1.000000000000000000, 1.371829164384562918E-16, 0.000000000000000000 ) ) ;
#436 = CARTESIAN_POINT ( 'NONE',  ( 42.50000000000000711, -12.00000000000012434, 47.50000000000000711 ) ) ;
#437 = EDGE_LOOP ( 'NONE', ( #19321, #11587 ) ) ;
#438 = B_SPLINE_CURVE_WITH_KNOTS ( 'NONE', 3,
 ( #10429, #22613, #10094, #4956, #5079, #11935, #22, #18935, #120, #7012, #15588, #17091, #13969, #17204, #1404, #1517, #19051, #3358, #20993, #10316, #17312, #5297, #12272, #19735 ),
 .UNSPECIFIED., .F., .F.,
 ( 4, 2, 2, 2, 2, 2, 2, 2, 2, 2, 2, 4 ),
 ( 0.02614117015034099489, 0.02729036340605310237, 0.02843955666176521332, 0.03073794317318943869, 0.03188713642890154965, 0.03303632968461366060, 0.03533471619603787556, 0.03648390945174998651, 0.03763310270746209746, 0.03993148921888632630, 0.04222987573031054820, 0.04452826224173477704 ),
 .UNSPECIFIED. ) ;
#439 = FACE_OUTER_BOUND ( 'NONE', #4503, .T. ) ;
#440 = DIRECTION ( 'NONE',  ( 0.000000000000000000, 1.000000000000000000, 0.000000000000000000 ) ) ;
#441 = DIRECTION ( 'NONE',  ( 0.000000000000000000, 0.000000000000000000, -1.000000000000000000 ) ) ;
#442 = AXIS2_PLACEMENT_3D ( 'NONE', #3968, #12531, #11161 ) ;
#443 = EDGE_CURVE ( 'NONE', #2350, #18209, #20357, .T. ) ;
#444 = ORIENTED_EDGE ( 'NONE', *, *, #19808, .F. ) ;
#445 = CARTESIAN_POINT ( 'NONE',  ( -15.12081897056664914, 33.51030287062364721, -2.800654218530457484 ) ) ;
#446 = ADVANCED_FACE ( 'NONE', ( #9810 ), #21783, .T. ) ;
#447 = ORIENTED_EDGE ( 'NONE', *, *, #13329, .T. ) ;
#448 = CARTESIAN_POINT ( 'NONE',  ( -4.170748987303213084, 34.65667543218822999, 3.000000000000002665 ) ) ;
#449 = CARTESIAN_POINT ( 'NONE',  ( -42.50000000000000711, -9.600000000000001421, -47.50000000000000000 ) ) ;
#450 = FACE_OUTER_BOUND ( 'NONE', #22695, .T. ) ;
#451 = ORIENTED_EDGE ( 'NONE', *, *, #20783, .T. ) ;
#452 = DIRECTION ( 'NONE',  ( -0.000000000000000000, -1.000000000000000000, -0.000000000000000000 ) ) ;
#453 = CARTESIAN_POINT ( 'NONE',  ( -9.689843208404424146, 39.33333333333333570, 54.54983754392744544 ) ) ;
#454 = VERTEX_POINT ( 'NONE', #9919 ) ;
#455 = CYLINDRICAL_SURFACE ( 'NONE', #13115, 25.00000000000000000 ) ;
#456 = CARTESIAN_POINT ( 'NONE',  ( 2.775557561562891351E-14, -2.775557561562891351E-14, 2.999999999999999112 ) ) ;
#457 = DIRECTION ( 'NONE',  ( 1.296372316667914327E-16, 1.000000000000000000, -0.000000000000000000 ) ) ;
#458 = AXIS2_PLACEMENT_3D ( 'NONE', #18438, #22003, #1140 ) ;
#459 = CARTESIAN_POINT ( 'NONE',  ( 8.206546567640634603E-16, -5.025303850726727362, 0.000000000000000000 ) ) ;
#460 = ORIENTED_EDGE ( 'NONE', *, *, #7404, .T. ) ;
#461 = CARTESIAN_POINT ( 'NONE',  ( 7.463862311151453710, 35.99819890246943999, -2.800654218530457484 ) ) ;
#462 = DIRECTION ( 'NONE',  ( 0.000000000000000000, -0.000000000000000000, 1.000000000000000000 ) ) ;
#463 = B_SPLINE_CURVE_WITH_KNOTS ( 'NONE', 3,
 ( #3611, #20792, #8757, #8523 ),
 .UNSPECIFIED., .F., .F.,
 ( 4, 4 ),
 ( 9.715086409175039034E-07, 0.001929643240672277446 ),
 .UNSPECIFIED. ) ;
#464 = CARTESIAN_POINT ( 'NONE',  ( -0.8008185833748354687, 39.99628548823710616, -49.34729503705691656 ) ) ;
#465 = EDGE_LOOP ( 'NONE', ( #20901, #7728 ) ) ;
#466 = FACE_OUTER_BOUND ( 'NONE', #16645, .T. ) ;
#467 = CARTESIAN_POINT ( 'NONE',  ( 31.21605069118074738, 8.646032897228984382, 2.999999999999995559 ) ) ;
#468 = DIRECTION ( 'NONE',  ( 0.000000000000000000, 1.000000000000000000, 0.000000000000000000 ) ) ;
#469 = EDGE_CURVE ( 'NONE', #19954, #548, #5572, .T. ) ;
#470 = ORIENTED_EDGE ( 'NONE', *, *, #21249, .T. ) ;
#471 = VECTOR ( 'NONE', #14248, 1000.000000000000000 ) ;
#472 = ORIENTED_EDGE ( 'NONE', *, *, #15222, .T. ) ;
#473 = EDGE_LOOP ( 'NONE', ( #18170, #2329, #19189, #6844 ) ) ;
#474 = CONICAL_SURFACE ( 'NONE', #18047, 58.99999999999701572, 0.7853981633974447263 ) ;
#475 =( NAMED_UNIT ( * ) SI_UNIT ( $, .STERADIAN. ) SOLID_ANGLE_UNIT ( ) );
#476 = EDGE_CURVE ( 'NONE', #15630, #19286, #14390, .T. ) ;
#477 = CIRCLE ( 'NONE', #13626, 2.099999999999997868 ) ;
#478 = VERTEX_POINT ( 'NONE', #4882 ) ;
#479 = CYLINDRICAL_SURFACE ( 'NONE', #15776, 2.099999999999997868 ) ;
#480 = LINE ( 'NONE', #7251, #20898 ) ;
#481 = CARTESIAN_POINT ( 'NONE',  ( 2.775557561562891351E-14, -2.775557561562891351E-14, 2.999999999999999112 ) ) ;
#482 = ORIENTED_EDGE ( 'NONE', *, *, #4999, .F. ) ;
#483 = CARTESIAN_POINT ( 'NONE',  ( -31.92986134326225667, 18.22261011550274645, 2.800654218530509443 ) ) ;
#484 = DIRECTION ( 'NONE',  ( -0.9898477157360406897, 0.000000000000000000, -0.1421319796954317316 ) ) ;
#485 = ORIENTED_EDGE ( 'NONE', *, *, #11304, .F. ) ;
#486 = CARTESIAN_POINT ( 'NONE',  ( -3.709350152758254637, -1.139907008998718663, 50.71254743501651063 ) ) ;
#487 = DIRECTION ( 'NONE',  ( 0.000000000000000000, 1.000000000000000000, 0.000000000000000000 ) ) ;
#488 = LINE ( 'NONE', #7485, #991 ) ;
#489 = ORIENTED_EDGE ( 'NONE', *, *, #9326, .F. ) ;
#490 = CARTESIAN_POINT ( 'NONE',  ( 2.951378045146772156, -1.204966337759544759, 50.23352299313199154 ) ) ;
#491 = ORIENTED_EDGE ( 'NONE', *, *, #16782, .F. ) ;
#492 = DIRECTION ( 'NONE',  ( -1.000000000000000000, -1.052817288873011806E-14, 0.000000000000000000 ) ) ;
#493 = CARTESIAN_POINT ( 'NONE',  ( 47.83731665821558465, 6.999999999999999112, 38.93845529828710283 ) ) ;
#494 = CARTESIAN_POINT ( 'NONE',  ( 3.849727973822421485E-15, 1.499999999999994449, 0.000000000000000000 ) ) ;
#495 = ORIENTED_EDGE ( 'NONE', *, *, #11690, .T. ) ;
#496 = CARTESIAN_POINT ( 'NONE',  ( 9.433064893952842311, 39.99999999999999289, -53.48670810797406006 ) ) ;
#497 = AXIS2_PLACEMENT_3D ( 'NONE', #8009, #16823, #14964 ) ;
#498 = CARTESIAN_POINT ( 'NONE',  ( 20.00279574339558053, 20.27588806490328466, 58.14815718762942254 ) ) ;
#499 = CARTESIAN_POINT ( 'NONE',  ( -15.49999999999980282, -2.516660498395516310, -105.0000000000000142 ) ) ;
#500 = CIRCLE ( 'NONE', #12915, 49.99999999999998579 ) ;
#501 = EDGE_CURVE ( 'NONE', #11241, #8065, #19539, .T. ) ;
#502 = AXIS2_PLACEMENT_3D ( 'NONE', #8254, #6205, #22245 ) ;
#503 = DIRECTION ( 'NONE',  ( 0.000000000000000000, 0.000000000000000000, -1.000000000000000000 ) ) ;
#504 = EDGE_CURVE ( 'NONE', #4461, #15820, #3176, .T. ) ;
#505 = ORIENTED_EDGE ( 'NONE', *, *, #18677, .F. ) ;
#506 = CIRCLE ( 'NONE', #7080, 2.500000000000002220 ) ;
#507 = VERTEX_POINT ( 'NONE', #8099 ) ;
#508 = ORIENTED_EDGE ( 'NONE', *, *, #14045, .T. ) ;
#509 = ORIENTED_EDGE ( 'NONE', *, *, #13212, .T. ) ;
#510 = DIRECTION ( 'NONE',  ( 0.000000000000000000, 0.000000000000000000, 1.000000000000000000 ) ) ;
#511 = DIRECTION ( 'NONE',  ( 0.000000000000000000, 0.000000000000000000, 1.000000000000000000 ) ) ;
#512 = VECTOR ( 'NONE', #9586, 1000.000000000000000 ) ;
#513 = DIRECTION ( 'NONE',  ( 0.000000000000000000, 0.000000000000000000, -1.000000000000000000 ) ) ;
#514 = B_SPLINE_CURVE_WITH_KNOTS ( 'NONE', 3,
 ( #8417, #8302, #13318, #978, #8189, #9907, #4423, #14934, #20459, #1094, #8087, #15044, #13658, #22301, #18383, #11517, #6251, #4767, #6589, #13209, #1429, #17113 ),
 .UNSPECIFIED., .F., .F.,
 ( 4, 2, 2, 2, 2, 2, 2, 2, 2, 2, 4 ),
 ( 0.000000000000000000, 0.1249999999999998612, 0.2499999999999997224, 0.3749999999999995559, 0.4374999999999996114, 0.4999999999999996669, 0.6249999999999996669, 0.7499999999999995559, 0.8749999999999995559, 0.9374999999999998890, 1.000000000000000000 ),
 .UNSPECIFIED. ) ;
#515 = ORIENTED_EDGE ( 'NONE', *, *, #6519, .F. ) ;
#516 = CARTESIAN_POINT ( 'NONE',  ( -34.99999999999999289, 0.000000000000000000, -3.012171160963566127E-14 ) ) ;
#517 = DIRECTION ( 'NONE',  ( 1.296372316667914327E-16, 1.000000000000000000, -0.000000000000000000 ) ) ;
#518 = VECTOR ( 'NONE', #17062, 1000.000000000000000 ) ;
#519 = EDGE_CURVE ( 'NONE', #5408, #3873, #7462, .T. ) ;
#520 = EDGE_CURVE ( 'NONE', #4189, #4363, #18750, .T. ) ;
#521 = EDGE_LOOP ( 'NONE', ( #7198, #21229, #17440, #9818 ) ) ;
#522 = DIRECTION ( 'NONE',  ( 1.296372316667914327E-16, 1.000000000000000000, -0.000000000000000000 ) ) ;
#523 = CARTESIAN_POINT ( 'NONE',  ( -42.50000000000000711, -5.000000000000000000, -45.40000000000000568 ) ) ;
#524 = FACE_OUTER_BOUND ( 'NONE', #18019, .T. ) ;
#525 = DIRECTION ( 'NONE',  ( -1.000000000000000000, 0.000000000000000000, 0.000000000000000000 ) ) ;
#526 =( REPRESENTATION_RELATIONSHIP ('NONE','NONE', #8442, #3430 ) REPRESENTATION_RELATIONSHIP_WITH_TRANSFORMATION ( #3107 )SHAPE_REPRESENTATION_RELATIONSHIP( ) );
#527 = EDGE_CURVE ( 'NONE', #21131, #15970, #924, .T. ) ;
#528 = VECTOR ( 'NONE', #1528, 1000.000000000000000 ) ;
#529 = CARTESIAN_POINT ( 'NONE',  ( 42.50000000000000711, -12.00000000000000000, 47.50000000000000711 ) ) ;
#530 = DIRECTION ( 'NONE',  ( 0.000000000000000000, -0.000000000000000000, -1.000000000000000000 ) ) ;
#531 = FACE_OUTER_BOUND ( 'NONE', #18877, .T. ) ;
#532 = CYLINDRICAL_SURFACE ( 'NONE', #9399, 30.00000000000000000 ) ;
#533 = AXIS2_PLACEMENT_3D ( 'NONE', #17654, #5513, #15925 ) ;
#534 = ORIENTED_EDGE ( 'NONE', *, *, #12604, .F. ) ;
#535 = EDGE_LOOP ( 'NONE', ( #8078, #13018, #9083, #19228 ) ) ;
#536 = ORIENTED_EDGE ( 'NONE', *, *, #10840, .T. ) ;
#537 = DIRECTION ( 'NONE',  ( -0.000000000000000000, 1.000000000000000000, -0.000000000000000000 ) ) ;
#538 = CIRCLE ( 'NONE', #12595, 15.00000000000000000 ) ;
#539 = CARTESIAN_POINT ( 'NONE',  ( -1.247165098465854882, 0.02902681952929966891, -51.42818515578048277 ) ) ;
#540 = EDGE_CURVE ( 'NONE', #20205, #18632, #21256, .T. ) ;
#541 = AXIS2_PLACEMENT_3D ( 'NONE', #5026, #15537, #8566 ) ;
#542 = CARTESIAN_POINT ( 'NONE',  ( 1.568459684869332627, 13.32608676514834301, 6.880481854261958574 ) ) ;
#543 = DIRECTION ( 'NONE',  ( 0.000000000000000000, 0.000000000000000000, 1.000000000000000000 ) ) ;
#544 = DIRECTION ( 'NONE',  ( -0.000000000000000000, 1.000000000000000000, -0.000000000000000000 ) ) ;
#545 = CARTESIAN_POINT ( 'NONE',  ( -10.79594548525845354, 39.62239930148190581, -54.90840750699925366 ) ) ;
#546 = FACE_OUTER_BOUND ( 'NONE', #6799, .T. ) ;
#547 = DIRECTION ( 'NONE',  ( -0.000000000000000000, 1.000000000000000000, -0.000000000000000000 ) ) ;
#548 = VERTEX_POINT ( 'NONE', #54 ) ;
#549 = EDGE_CURVE ( 'NONE', #21392, #4403, #13704, .T. ) ;
#550 = FACE_OUTER_BOUND ( 'NONE', #1337, .T. ) ;
#551 = CARTESIAN_POINT ( 'NONE',  ( -1.387778780781445676E-14, 40.00000000000000000, -48.73397172404481381 ) ) ;
#552 = FACE_BOUND ( 'NONE', #22629, .T. ) ;
#553 = AXIS2_PLACEMENT_3D ( 'NONE', #10105, #20446, #6915 ) ;
#554 = CARTESIAN_POINT ( 'NONE',  ( 7.033428926742989695, 6.687309450572964664, -41.47353357286041842 ) ) ;
#555 = ORIENTED_EDGE ( 'NONE', *, *, #20018, .F. ) ;
#556 = PLANE ( 'NONE',  #2500 ) ;
#557 = CIRCLE ( 'NONE', #3135, 31.50000000000000711 ) ;
#558 = ORIENTED_EDGE ( 'NONE', *, *, #1941, .T. ) ;
#559 = DIRECTION ( 'NONE',  ( 1.000000000000000000, 0.000000000000000000, 0.000000000000000000 ) ) ;
#560 = CARTESIAN_POINT ( 'NONE',  ( -1.387778780781445676E-14, 20.00000000000000000, -100.0000000000000000 ) ) ;
#561 = EDGE_CURVE ( 'NONE', #19756, #19564, #12445, .T. ) ;
#562 = AXIS2_PLACEMENT_3D ( 'NONE', #8192, #22408, #11628 ) ;
#563 = ORIENTED_EDGE ( 'NONE', *, *, #5695, .F. ) ;
#564 = CARTESIAN_POINT ( 'NONE',  ( 14.99999999999998579, 20.00000000000000355, 60.00200000000000244 ) ) ;
#565 = ADVANCED_FACE ( 'NONE', ( #8537 ), #7046, .F. ) ;
#566 = DIRECTION ( 'NONE',  ( 0.000000000000000000, 0.000000000000000000, -1.000000000000000000 ) ) ;
#567 = CIRCLE ( 'NONE', #13356, 0.9999999999999974465 ) ;
#568 = ORIENTED_EDGE ( 'NONE', *, *, #3531, .T. ) ;
#569 = CARTESIAN_POINT ( 'NONE',  ( -13.85640646055084702, -1.500000000000011768, 11.99999999999970335 ) ) ;
#570 = CIRCLE ( 'NONE', #3154, 19.99999999999999289 ) ;
#571 = CYLINDRICAL_SURFACE ( 'NONE', #12438, 36.76383501243555685 ) ;
#572 = DIRECTION ( 'NONE',  ( 0.000000000000000000, 0.000000000000000000, -1.000000000000000000 ) ) ;
#573 = VERTEX_POINT ( 'NONE', #3286 ) ;
#574 = CARTESIAN_POINT ( 'NONE',  ( 35.00000000000000000, 22.00000000000000355, 17.00000000000002487 ) ) ;
#575 = VERTEX_POINT ( 'NONE', #17585 ) ;
#576 = DIRECTION ( 'NONE',  ( -0.000000000000000000, 1.000000000000000000, -0.000000000000000000 ) ) ;
#577 = AXIS2_PLACEMENT_3D ( 'NONE', #19256, #1, #8819 ) ;
#578 = DIRECTION ( 'NONE',  ( 0.000000000000000000, 0.000000000000000000, 1.000000000000000000 ) ) ;
#579 = CARTESIAN_POINT ( 'NONE',  ( -9.064496942927510403, 40.00000000000000711, 53.36141823319849919 ) ) ;
#580 = VECTOR ( 'NONE', #14375, 1000.000000000000000 ) ;
#581 = DIRECTION ( 'NONE',  ( -6.505213034913038160E-19, -3.903127820947822896E-18, -1.000000000000000000 ) ) ;
#582 = EDGE_LOOP ( 'NONE', ( #20787, #19014, #14328, #6935, #11159 ) ) ;
#583 = DIRECTION ( 'NONE',  ( 6.505213034913038160E-19, 3.903127820947822896E-18, 1.000000000000000000 ) ) ;
#584 = DIRECTION ( 'NONE',  ( 1.000000000000000000, 0.000000000000000000, 0.000000000000000000 ) ) ;
#585 = CARTESIAN_POINT ( 'NONE',  ( -0.6551157041172263051, 39.99751803486232404, -49.23722055247538520 ) ) ;
#586 = VERTEX_POINT ( 'NONE', #3393 ) ;
#587 = DIRECTION ( 'NONE',  ( 1.000000000000000000, 0.000000000000000000, 0.000000000000000000 ) ) ;
#588 = CARTESIAN_POINT ( 'NONE',  ( -6.261274683082161729, 0.9579800028911584775, 54.84444022978226485 ) ) ;
#589 = AXIS2_PLACEMENT_3D ( 'NONE', #14454, #144, #14110 ) ;
#590 = EDGE_CURVE ( 'NONE', #6177, #19116, #506, .T. ) ;
#591 = CIRCLE ( 'NONE', #19618, 34.90673715956759082 ) ;
#592 = AXIS2_PLACEMENT_3D ( 'NONE', #3774, #3673, #10624 ) ;
#593 = ORIENTED_EDGE ( 'NONE', *, *, #20919, .F. ) ;
#594 = EDGE_CURVE ( 'NONE', #9609, #19656, #19896, .T. ) ;
#595 = CIRCLE ( 'NONE', #3894, 10.00000000000000000 ) ;
#596 = EDGE_LOOP ( 'NONE', ( #6630, #2604, #22575, #5586 ) ) ;
#597 = ORIENTED_EDGE ( 'NONE', *, *, #20910, .T. ) ;
#598 =( LENGTH_UNIT ( ) NAMED_UNIT ( * ) SI_UNIT ( .MILLI., .METRE. ) );
#599 = VERTEX_POINT ( 'NONE', #15846 ) ;
#600 = CARTESIAN_POINT ( 'NONE',  ( 32.09841355225995585, -5.093313992686393732, -2.999999999999971578 ) ) ;
#601 = DIRECTION ( 'NONE',  ( -6.505213034913038160E-19, -3.903127820947822896E-18, -1.000000000000000000 ) ) ;
#602 = CARTESIAN_POINT ( 'NONE',  ( 25.00000000000000000, -20.00000000000000000, 6.487780019669002523E-15 ) ) ;
#603 = ORIENTED_EDGE ( 'NONE', *, *, #21489, .T. ) ;
#604 = CARTESIAN_POINT ( 'NONE',  ( -26.00000000000001421, 19.99999999999982947, 105.0000000000000142 ) ) ;
#605 = CARTESIAN_POINT ( 'NONE',  ( -26.00000000000001421, 19.99999999999982947, -105.0000000000000142 ) ) ;
#606 = ORIENTED_EDGE ( 'NONE', *, *, #5866, .F. ) ;
#607 = DIRECTION ( 'NONE',  ( 0.000000000000000000, 0.000000000000000000, 1.000000000000000000 ) ) ;
#608 = AXIS2_PLACEMENT_3D ( 'NONE', #8171, #20770, #9889 ) ;
#609 = CARTESIAN_POINT ( 'NONE',  ( -42.50000000000000711, -12.00000000000000000, 45.40000000000001279 ) ) ;
#610 = DIRECTION ( 'NONE',  ( 1.000000000000000000, -1.301042606982605814E-16, 0.000000000000000000 ) ) ;
#611 = ORIENTED_EDGE ( 'NONE', *, *, #4266, .F. ) ;
#612 = EDGE_CURVE ( 'NONE', #4064, #19773, #10257, .T. ) ;
#613 = CARTESIAN_POINT ( 'NONE',  ( 5.511499161255899004, 0.6970817516857953366, 52.42185088604356480 ) ) ;
#614 = ORIENTED_EDGE ( 'NONE', *, *, #18115, .T. ) ;
#615 = CARTESIAN_POINT ( 'NONE',  ( 6.450208405384564081, 39.75599223657528825, 53.02618523645297444 ) ) ;
#616 = FACE_OUTER_BOUND ( 'NONE', #2436, .T. ) ;
#617 = AXIS2_PLACEMENT_3D ( 'NONE', #4326, #16459, #11301 ) ;
#618 = ORIENTED_EDGE ( 'NONE', *, *, #4093, .F. ) ;
#619 = CARTESIAN_POINT ( 'NONE',  ( -1.387778780781445676E-14, 20.00000000000000000, 100.0000000000000000 ) ) ;
#620 = CARTESIAN_POINT ( 'NONE',  ( -23.50000000000001066, 19.99999999999982947, 100.0000000000000000 ) ) ;
#621 = EDGE_CURVE ( 'NONE', #21949, #5947, #10354, .T. ) ;
#622 = EDGE_CURVE ( 'NONE', #14783, #19446, #2359, .T. ) ;
#623 = DIRECTION ( 'NONE',  ( 0.000000000000000000, 0.000000000000000000, -1.000000000000000000 ) ) ;
#624 = AXIS2_PLACEMENT_3D ( 'NONE', #14990, #8139, #11902 ) ;
#625 = ORIENTED_EDGE ( 'NONE', *, *, #14576, .T. ) ;
#626 = VERTEX_POINT ( 'NONE', #3731 ) ;
#627 = ORIENTED_EDGE ( 'NONE', *, *, #19282, .F. ) ;
#628 = ORIENTED_EDGE ( 'NONE', *, *, #16506, .F. ) ;
#629 = CARTESIAN_POINT ( 'NONE',  ( -90.00000000000000000, 40.00000000000000000, 2.500000000000001332 ) ) ;
#630 = DIRECTION ( 'NONE',  ( 0.000000000000000000, -1.000000000000000000, 0.000000000000000000 ) ) ;
#631 = DIRECTION ( 'NONE',  ( -0.000000000000000000, -1.000000000000000000, -0.000000000000000000 ) ) ;
#632 = ORIENTED_EDGE ( 'NONE', *, *, #6395, .T. ) ;
#633 = CARTESIAN_POINT ( 'NONE',  ( 21.00948735876884044, 24.79619811426203668, -6.999999999999950262 ) ) ;
#634 = CARTESIAN_POINT ( 'NONE',  ( 90.00000000000000000, 26.00000000000000355, 2.099999999999989875 ) ) ;
#635 = VECTOR ( 'NONE', #1063, 1000.000000000000114 ) ;
#636 = B_SPLINE_CURVE_WITH_KNOTS ( 'NONE', 3,
 ( #6378, #17250, #4785, #15175, #18648, #11867, #2952, #18868, #17137, #1455, #1560, #9926, #1216, #22200, #6493, #19858 ),
 .UNSPECIFIED., .F., .F.,
 ( 4, 2, 2, 2, 2, 2, 2, 4 ),
 ( 0.000000000000000000, 0.004782611835060888474, 0.005978264793826106906, 0.007173917752591319266, 0.009565223670121737048, 0.01195652958765215483, 0.01434783550518257435, 0.01913044734024341512 ),
 .UNSPECIFIED. ) ;
#637 = EDGE_CURVE ( 'NONE', #15664, #18218, #10005, .T. ) ;
#638 = EDGE_LOOP ( 'NONE', ( #7057, #3498, #13428, #19774 ) ) ;
#639 = CARTESIAN_POINT ( 'NONE',  ( 42.50000000000000000, 7.000000000000000000, 49.99999999999999289 ) ) ;
#640 = CIRCLE ( 'NONE', #11227, 2.499999999999995115 ) ;
#641 = CARTESIAN_POINT ( 'NONE',  ( -42.50000000000000711, -5.000000000000000000, 41.00000000000000711 ) ) ;
#642 = CARTESIAN_POINT ( 'NONE',  ( 90.00000000000000000, 26.00000000000000355, -2.099999999999991651 ) ) ;
#643 = AXIS2_PLACEMENT_3D ( 'NONE', #1476, #22451, #1241 ) ;
#644 = CARTESIAN_POINT ( 'NONE',  ( -22.12933039895921183, -2.999999999999992895, 0.000000000000000000 ) ) ;
#645 = EDGE_CURVE ( 'NONE', #4303, #9582, #20624, .T. ) ;
#646 = EDGE_CURVE ( 'NONE', #11081, #11262, #14027, .T. ) ;
#647 = DIRECTION ( 'NONE',  ( 0.000000000000000000, 0.000000000000000000, -1.000000000000000000 ) ) ;
#648 = AXIS2_PLACEMENT_3D ( 'NONE', #22157, #18941, #22389 ) ;
#649 = DIRECTION ( 'NONE',  ( 1.000000000000000000, 0.000000000000000000, 0.000000000000000000 ) ) ;
#650 = EDGE_CURVE ( 'NONE', #2517, #14456, #15130, .T. ) ;
#651 = VERTEX_POINT ( 'NONE', #17468 ) ;
#652 = AXIS2_PLACEMENT_3D ( 'NONE', #13595, #1481, #11895 ) ;
#653 = EDGE_LOOP ( 'NONE', ( #11685, #3181, #17197, #9101 ) ) ;
#654 = VECTOR ( 'NONE', #4707, 1000.000000000000000 ) ;
#655 = ADVANCED_FACE ( 'NONE', ( #1789 ), #15745, .T. ) ;
#656 = AXIS2_PLACEMENT_3D ( 'NONE', #1334, #18751, #13229 ) ;
#657 = EDGE_LOOP ( 'NONE', ( #17524, #9089, #7383, #7095 ) ) ;
#658 = DIRECTION ( 'NONE',  ( 0.000000000000000000, 0.000000000000000000, 1.000000000000000000 ) ) ;
#659 = CARTESIAN_POINT ( 'NONE',  ( 4.000000000000003553, -1.500000000000015099, 0.000000000000000000 ) ) ;
#660 = AXIS2_PLACEMENT_3D ( 'NONE', #764, #11299, #10833 ) ;
#661 = FACE_OUTER_BOUND ( 'NONE', #1127, .T. ) ;
#662 = FACE_OUTER_BOUND ( 'NONE', #3144, .T. ) ;
#663 = CARTESIAN_POINT ( 'NONE',  ( 6.699391982047661287, -4.821764332415560794, 49.69317737456783846 ) ) ;
#664 = DIRECTION ( 'NONE',  ( 0.000000000000000000, 1.000000000000000000, 0.000000000000000000 ) ) ;
#665 = CARTESIAN_POINT ( 'NONE',  ( -10.70799354677358295, 35.16985127952384715, -2.800654218530457484 ) ) ;
#666 = AXIS2_PLACEMENT_3D ( 'NONE', #5556, #12535, #9120 ) ;
#667 = VECTOR ( 'NONE', #15836, 1000.000000000000000 ) ;
#668 = VERTEX_POINT ( 'NONE', #2002 ) ;
#669 = CIRCLE ( 'NONE', #11643, 22.12933039895921539 ) ;
#670 = DIRECTION ( 'NONE',  ( -1.000000000000000000, 0.000000000000000000, 0.000000000000000000 ) ) ;
#671 = DIRECTION ( 'NONE',  ( -0.000000000000000000, -0.000000000000000000, 1.000000000000000000 ) ) ;
#672 = CARTESIAN_POINT ( 'NONE',  ( 34.99999999999999289, 0.000000000000000000, -57.49999999999705835 ) ) ;
#673 = DIRECTION ( 'NONE',  ( -6.505213034913038160E-19, -3.903127820947822896E-18, -1.000000000000000000 ) ) ;
#674 = AXIS2_PLACEMENT_3D ( 'NONE', #11250, #20311, #16409 ) ;
#675 = VERTEX_POINT ( 'NONE', #8986 ) ;
#676 = ORIENTED_EDGE ( 'NONE', *, *, #4878, .T. ) ;
#677 = DIRECTION ( 'NONE',  ( -0.000000000000000000, -0.000000000000000000, -1.000000000000000000 ) ) ;
#678 = CARTESIAN_POINT ( 'NONE',  ( -35.00000000000000000, -9.000000000000001776, -17.99999999999998934 ) ) ;
#679 = ADVANCED_FACE ( 'NONE', ( #11272 ), #21599, .F. ) ;
#680 = EDGE_CURVE ( 'NONE', #9888, #4267, #16975, .T. ) ;
#681 = B_SPLINE_CURVE_WITH_KNOTS ( 'NONE', 1,
 ( #16046, #17548 ),
 .UNSPECIFIED., .F., .F.,
 ( 2, 2 ),
 ( 0.000000000000000000, 1.000000000000000000 ),
 .UNSPECIFIED. ) ;
#682 = AXIS2_PLACEMENT_3D ( 'NONE', #13089, #4934, #8373 ) ;
#683 = AXIS2_PLACEMENT_3D ( 'NONE', #20759, #3350, #19155 ) ;
#684 = ORIENTED_EDGE ( 'NONE', *, *, #8709, .F. ) ;
#685 = CONICAL_SURFACE ( 'NONE', #20455, 2.099999999999997868, 1.029744258676653867 ) ;
#686 = LINE ( 'NONE', #5725, #14759 ) ;
#687 = CIRCLE ( 'NONE', #13469, 19.11328065563150957 ) ;
#688 = EDGE_CURVE ( 'NONE', #6587, #2221, #21014, .T. ) ;
#689 = CARTESIAN_POINT ( 'NONE',  ( -4.153395668489446635, 35.29097153256767427, -3.000000000000005773 ) ) ;
#690 = VECTOR ( 'NONE', #4946, 1000.000000000000000 ) ;
#691 = VERTEX_POINT ( 'NONE', #19537 ) ;
#692 = CARTESIAN_POINT ( 'NONE',  ( 1.105958719418588032, 39.99272030489618857, -49.57516106150625035 ) ) ;
#693 = CARTESIAN_POINT ( 'NONE',  ( 35.00000000000000000, 15.00000000000000000, -40.99999999999997868 ) ) ;
#694 = DIRECTION ( 'NONE',  ( 1.296372316667914327E-16, 1.000000000000000000, -0.000000000000000000 ) ) ;
#695 = EDGE_LOOP ( 'NONE', ( #15730, #4327, #172, #15716, #13591, #19027, #8915 ) ) ;
#696 = CARTESIAN_POINT ( 'NONE',  ( 42.50000000000000711, -11.97499999999999964, 50.00000000000000711 ) ) ;
#697 = CARTESIAN_POINT ( 'NONE',  ( -9.867969867547959240, 0.2954100743916240890, -54.30456930252523051 ) ) ;
#698 = EDGE_LOOP ( 'NONE', ( #8656, #15794, #19959, #10887 ) ) ;
#699 = LINE ( 'NONE', #7682, #18205 ) ;
#700 = CARTESIAN_POINT ( 'NONE',  ( 2.220446049250313081E-13, -8.326672684688674053E-14, 2.800654218530498785 ) ) ;
#701 = CYLINDRICAL_SURFACE ( 'NONE', #14041, 2.500000000000002220 ) ;
#702 = CIRCLE ( 'NONE', #18268, 41.25806096964026892 ) ;
#703 = ORIENTED_EDGE ( 'NONE', *, *, #22176, .T. ) ;
#704 = CARTESIAN_POINT ( 'NONE',  ( -5.999999999999998224, -20.00000000000000000, 5.999999999999999112 ) ) ;
#705 = FACE_OUTER_BOUND ( 'NONE', #13898, .T. ) ;
#706 = AXIS2_PLACEMENT_3D ( 'NONE', #726, #7708, #376 ) ;
#707 = CARTESIAN_POINT ( 'NONE',  ( -0.09263077948485531898, 39.99995274011368451, -48.80595708259651389 ) ) ;
#708 = ORIENTED_EDGE ( 'NONE', *, *, #21758, .F. ) ;
#709 = DIRECTION ( 'NONE',  ( 0.000000000000000000, -0.5150380749100547106, -0.8571673007021120005 ) ) ;
#710 = ADVANCED_FACE ( 'NONE', ( #9559 ), #16194, .F. ) ;
#711 = CARTESIAN_POINT ( 'NONE',  ( -13.07600923154787864, 27.35939529837144590, 44.93756990742566870 ) ) ;
#712 = DIRECTION ( 'NONE',  ( 0.000000000000000000, 0.000000000000000000, 1.000000000000000000 ) ) ;
#713 = PRODUCT_DEFINITION_SHAPE ( 'NONE', 'NONE',  #22705 ) ;
#714 = ORIENTED_EDGE ( 'NONE', *, *, #18426, .F. ) ;
#715 = ORIENTED_EDGE ( 'NONE', *, *, #1941, .F. ) ;
#716 = CIRCLE ( 'NONE', #14971, 15.00000000000000000 ) ;
#717 = ORIENTED_EDGE ( 'NONE', *, *, #8304, .F. ) ;
#718 = SHAPE_REPRESENTATION_RELATIONSHIP ( 'NONE' , 'NONE' ,  #15726, #21138 ) ;
#719 = ORIENTED_EDGE ( 'NONE', *, *, #14828, .T. ) ;
#720 = CARTESIAN_POINT ( 'NONE',  ( 19.01465036493455685, 26.21927150370769510, 60.37937655616645571 ) ) ;
#721 = DIRECTION ( 'NONE',  ( -1.000000000000000000, -1.208970125616046080E-17, 6.505213034913038160E-19 ) ) ;
#722 = CARTESIAN_POINT ( 'NONE',  ( -2.673152730111970410, 23.56975547524771741, 8.612623190900162484 ) ) ;
#723 = DIRECTION ( 'NONE',  ( 0.000000000000000000, 1.000000000000000000, -0.000000000000000000 ) ) ;
#724 = CARTESIAN_POINT ( 'NONE',  ( 35.00000000000000000, 0.000000000000000000, -49.99999999999997868 ) ) ;
#725 = ORIENTED_EDGE ( 'NONE', *, *, #5057, .T. ) ;
#726 = CARTESIAN_POINT ( 'NONE',  ( -36.39375341857506641, -7.980461308160019307, 2.999999999999995559 ) ) ;
#727 = FACE_OUTER_BOUND ( 'NONE', #1242, .T. ) ;
#728 = VERTEX_POINT ( 'NONE', #12980 ) ;
#729 = CARTESIAN_POINT ( 'NONE',  ( 34.99999999999980815, 26.00000000000000355, 57.09999999999921982 ) ) ;
#730 = EDGE_CURVE ( 'NONE', #17893, #10226, #5782, .T. ) ;
#731 = CARTESIAN_POINT ( 'NONE',  ( -20.67483659015370989, 11.23071942442636661, -58.26617649125748954 ) ) ;
#732 = PRODUCT_RELATED_PRODUCT_CATEGORY ( 'part', '', ( #1799 ) ) ;
#733 = DIRECTION ( 'NONE',  ( 0.000000000000000000, 0.000000000000000000, -1.000000000000000000 ) ) ;
#734 = ORIENTED_EDGE ( 'NONE', *, *, #2868, .F. ) ;
#735 = CARTESIAN_POINT ( 'NONE',  ( 3.330669073875469621E-13, -1.110223024625156540E-13, -2.999999999999971578 ) ) ;
#736 = CARTESIAN_POINT ( 'NONE',  ( 35.00000000000058265, 40.00000000000000000, -57.50000000000076028 ) ) ;
#737 = ORIENTED_EDGE ( 'NONE', *, *, #18385, .T. ) ;
#738 = CARTESIAN_POINT ( 'NONE',  ( 0.7832247060116511728, 40.00000000000097344, 49.34584201034998330 ) ) ;
#739 = DIRECTION ( 'NONE',  ( 6.505213034913038160E-19, 3.903127820947822896E-18, 1.000000000000000000 ) ) ;
#740 = EDGE_CURVE ( 'NONE', #9582, #4006, #18031, .T. ) ;
#741 = ORIENTED_EDGE ( 'NONE', *, *, #20768, .T. ) ;
#742 = CIRCLE ( 'NONE', #8713, 2.499999999999995115 ) ;
#743 = DIRECTION ( 'NONE',  ( -1.000000000000000000, 0.000000000000000000, 0.000000000000000000 ) ) ;
#744 = LINE ( 'NONE', #7724, #8894 ) ;
#745 = ORIENTED_EDGE ( 'NONE', *, *, #22049, .T. ) ;
#746 = AXIS2_PLACEMENT_3D ( 'NONE', #2751, #20166, #1139 ) ;
#747 = ORIENTED_EDGE ( 'NONE', *, *, #16037, .F. ) ;
#748 = EDGE_CURVE ( 'NONE', #17126, #21624, #7387, .T. ) ;
#749 = ORIENTED_EDGE ( 'NONE', *, *, #19224, .T. ) ;
#750 = ORIENTED_EDGE ( 'NONE', *, *, #2861, .F. ) ;
#751 = FACE_OUTER_BOUND ( 'NONE', #92, .T. ) ;
#752 = CARTESIAN_POINT ( 'NONE',  ( -35.00000000000000000, 17.00000000000000000, 41.00000000000002132 ) ) ;
#753 = DIRECTION ( 'NONE',  ( 0.000000000000000000, -0.000000000000000000, -1.000000000000000000 ) ) ;
#754 = ORIENTED_EDGE ( 'NONE', *, *, #3, .T. ) ;
#755 = CARTESIAN_POINT ( 'NONE',  ( -30.57187188083515750, -7.711478842616581453, -7.000000000000006217 ) ) ;
#756 = DIRECTION ( 'NONE',  ( -1.000000000000000000, -1.208970125616060717E-17, 0.000000000000000000 ) ) ;
#757 = ADVANCED_FACE ( 'NONE', ( #19874, #4184, #394, #12758, #16084, #21830, #9335 ), #6125, .T. ) ;
#758 = ORIENTED_EDGE ( 'NONE', *, *, #14920, .T. ) ;
#759 = DIRECTION ( 'NONE',  ( 0.000000000000000000, 1.000000000000000000, 0.000000000000000000 ) ) ;
#760 = FACE_OUTER_BOUND ( 'NONE', #5319, .T. ) ;
#761 = CYLINDRICAL_SURFACE ( 'NONE', #958, 2.500000000000002220 ) ;
#762 = DIRECTION ( 'NONE',  ( 0.000000000000000000, 1.000000000000000000, 0.000000000000000000 ) ) ;
#763 = LINE ( 'NONE', #21503, #19035 ) ;
#764 = CARTESIAN_POINT ( 'NONE',  ( 2.775557561562891351E-14, -2.775557561562891351E-14, 2.999999999999999112 ) ) ;
#765 = CARTESIAN_POINT ( 'NONE',  ( -1.387778780781445518E-14, 20.00000000000000355, -102.0000000000000142 ) ) ;
#766 = DIRECTION ( 'NONE',  ( 6.505213034913038160E-19, 3.903127820947822896E-18, 1.000000000000000000 ) ) ;
#767 = VERTEX_POINT ( 'NONE', #11155 ) ;
#768 = VERTEX_POINT ( 'NONE', #14807 ) ;
#769 = ADVANCED_FACE ( 'NONE', ( #14353 ), #18824, .F. ) ;
#770 = VECTOR ( 'NONE', #3039, 1000.000000000000114 ) ;
#771 = EDGE_LOOP ( 'NONE', ( #13106, #15939, #8345, #9673 ) ) ;
#772 = DIRECTION ( 'NONE',  ( -0.000000000000000000, -1.000000000000000000, -0.000000000000000000 ) ) ;
#773 = CARTESIAN_POINT ( 'NONE',  ( -18.00000000000001421, 20.00000000000000355, -102.9999999999999716 ) ) ;
#774 = CARTESIAN_POINT ( 'NONE',  ( 3.315551171827967991, 0.2472631163744288263, -51.08212483308732743 ) ) ;
#775 = EDGE_CURVE ( 'NONE', #15249, #1751, #7841, .T. ) ;
#776 = ADVANCED_FACE ( 'NONE', ( #12637 ), #12640, .F. ) ;
#777 = EDGE_CURVE ( 'NONE', #10435, #18495, #16621, .T. ) ;
#778 = DIRECTION ( 'NONE',  ( 0.000000000000000000, 0.000000000000000000, 1.000000000000000000 ) ) ;
#779 = CARTESIAN_POINT ( 'NONE',  ( -25.00000000000000000, -20.00000000000000000, 6.487780019669002523E-15 ) ) ;
#780 = CARTESIAN_POINT ( 'NONE',  ( -17.32050807568873196, -1.500000000000011768, 9.999999999999772626 ) ) ;
#781 = CARTESIAN_POINT ( 'NONE',  ( 3.330669073875469621E-13, -1.110223024625156540E-13, -2.999999999999971578 ) ) ;
#782 = FACE_OUTER_BOUND ( 'NONE', #19177, .T. ) ;
#783 = ORIENTED_EDGE ( 'NONE', *, *, #13913, .T. ) ;
#784 = DIRECTION ( 'NONE',  ( 6.505213034913038160E-19, 3.903127820947822896E-18, 1.000000000000000000 ) ) ;
#785 = EDGE_CURVE ( 'NONE', #21816, #1314, #14411, .T. ) ;
#786 = CARTESIAN_POINT ( 'NONE',  ( -6.401904815323844922, 38.95163572918602313, -55.13655742298576001 ) ) ;
#787 = CARTESIAN_POINT ( 'NONE',  ( 28.49999999999998224, 19.99999999999999645, 100.0000000000000000 ) ) ;
#788 = CARTESIAN_POINT ( 'NONE',  ( 12.99999999999999467, -20.00000000000000000, 11.32475165290614605 ) ) ;
#789 = EDGE_CURVE ( 'NONE', #1700, #2703, #7118, .T. ) ;
#790 = VERTEX_POINT ( 'NONE', #3368 ) ;
#791 = ORIENTED_EDGE ( 'NONE', *, *, #16352, .T. ) ;
#792 = CARTESIAN_POINT ( 'NONE',  ( 35.00000000000000000, 38.99999999999999289, -59.99999999999999289 ) ) ;
#793 = DIRECTION ( 'NONE',  ( 1.296372316667914327E-16, 1.000000000000000000, -0.000000000000000000 ) ) ;
#794 = EDGE_CURVE ( 'NONE', #10901, #12610, #2063, .T. ) ;
#795 = ORIENTED_EDGE ( 'NONE', *, *, #10962, .F. ) ;
#796 = CYLINDRICAL_SURFACE ( 'NONE', #18437, 2.099999999999997868 ) ;
#797 = AXIS2_PLACEMENT_3D ( 'NONE', #6808, #136, #18008 ) ;
#798 = CARTESIAN_POINT ( 'NONE',  ( 4.846088107612517959, 40.00000000000000000, -51.53252798484124497 ) ) ;
#799 = ORIENTED_EDGE ( 'NONE', *, *, #20849, .F. ) ;
#800 = CARTESIAN_POINT ( 'NONE',  ( 7.213743607555469950, 39.66007621396295946, -53.46062051868064202 ) ) ;
#801 = CARTESIAN_POINT ( 'NONE',  ( -31.41239365194187272, 2.347663744114131035, -2.999999999999999112 ) ) ;
#802 = FACE_OUTER_BOUND ( 'NONE', #3383, .T. ) ;
#803 = DIRECTION ( 'NONE',  ( 1.000000000000000000, 0.000000000000000000, 0.000000000000000000 ) ) ;
#804 = DIRECTION ( 'NONE',  ( -6.505213034913038160E-19, -3.903127820947822896E-18, -1.000000000000000000 ) ) ;
#805 = ADVANCED_FACE ( 'NONE', ( #10988 ), #3257, .T. ) ;
#806 = CARTESIAN_POINT ( 'NONE',  ( -6.910507445196895304, 40.00000000000002132, 52.51112221451682416 ) ) ;
#807 = ADVANCED_FACE ( 'NONE', ( #13643, #2280 ), #20659, .T. ) ;
#808 = CARTESIAN_POINT ( 'NONE',  ( -32.09841355225989901, 5.093313992686310243, -2.999999999999971578 ) ) ;
#809 = EDGE_LOOP ( 'NONE', ( #12173, #12291, #2991, #3318 ) ) ;
#810 = DIRECTION ( 'NONE',  ( 0.000000000000000000, 1.000000000000000000, 0.000000000000000000 ) ) ;
#811 = DIRECTION ( 'NONE',  ( 6.505213034913038160E-19, 3.903127820947822896E-18, 1.000000000000000000 ) ) ;
#812 = CARTESIAN_POINT ( 'NONE',  ( -0.02199734621860905542, 39.99999719748067406, -48.75108928016371124 ) ) ;
#813 = ORIENTED_EDGE ( 'NONE', *, *, #21249, .F. ) ;
#814 = AXIS2_PLACEMENT_3D ( 'NONE', #20289, #11347, #21901 ) ;
#815 = EDGE_CURVE ( 'NONE', #15823, #14245, #10221, .T. ) ;
#816 = LINE ( 'NONE', #2658, #1235 ) ;
#817 = VERTEX_POINT ( 'NONE', #7327 ) ;
#818 = ORIENTED_EDGE ( 'NONE', *, *, #18319, .T. ) ;
#819 = ORIENTED_EDGE ( 'NONE', *, *, #12527, .T. ) ;
#820 = CARTESIAN_POINT ( 'NONE',  ( 10.70799354677390269, -35.16985127952376899, -1.999999999999977573 ) ) ;
#821 = CARTESIAN_POINT ( 'NONE',  ( 5.748506628226523141, -0.6819283742239256041, 52.01451867725413081 ) ) ;
#822 = AXIS2_PLACEMENT_3D ( 'NONE', #1588, #15211, #10392 ) ;
#823 = CIRCLE ( 'NONE', #18392, 22.00000000000000000 ) ;
#824 = DIRECTION ( 'NONE',  ( -1.000000000000000000, -1.208970125616062874E-17, 0.000000000000000000 ) ) ;
#825 = DIRECTION ( 'NONE',  ( 1.049727191138617217E-16, 0.5150380749100562650, -0.8571673007021111124 ) ) ;
#826 = CARTESIAN_POINT ( 'NONE',  ( -34.99999999999980815, 40.00000000000000711, 54.99999999999922551 ) ) ;
#827 = ORIENTED_EDGE ( 'NONE', *, *, #19139, .F. ) ;
#828 = CARTESIAN_POINT ( 'NONE',  ( 9.952189117650823036, 40.00000000000000000, 53.64426396172073197 ) ) ;
#829 = FACE_OUTER_BOUND ( 'NONE', #20164, .T. ) ;
#830 = ORIENTED_EDGE ( 'NONE', *, *, #3767, .F. ) ;
#831 = CARTESIAN_POINT ( 'NONE',  ( -11.13407802442742245, 9.941921282207680122, -43.93745127716449872 ) ) ;
#832 = VECTOR ( 'NONE', #9450, 1000.000000000000000 ) ;
#833 = DIRECTION ( 'NONE',  ( 6.505213034913038160E-19, 3.903127820947822896E-18, 1.000000000000000000 ) ) ;
#834 = CARTESIAN_POINT ( 'NONE',  ( 19.04641992693177244, 13.69305383064222603, -60.38882653684736823 ) ) ;
#835 = ORIENTED_EDGE ( 'NONE', *, *, #6395, .F. ) ;
#836 = CARTESIAN_POINT ( 'NONE',  ( 36.75746821813308429, -0.6841746959067585010, 2.800654218530485018 ) ) ;
#837 = CARTESIAN_POINT ( 'NONE',  ( -42.49999999999996447, 10.00000000000000000, -54.00000000000000711 ) ) ;
#838 = EDGE_LOOP ( 'NONE', ( #3738, #12394, #3480, #9059 ) ) ;
#839 = CARTESIAN_POINT ( 'NONE',  ( 3.630513325115385381, 39.68566305962351493, 51.94955563033850865 ) ) ;
#840 = CARTESIAN_POINT ( 'NONE',  ( -0.2854126906103648387, -4.332981472378772736, -48.52899265465751455 ) ) ;
#841 = CARTESIAN_POINT ( 'NONE',  ( -6.001999869223751283, -0.8367338791974072709, -52.11627801855959063 ) ) ;
#842 = EDGE_LOOP ( 'NONE', ( #12632, #21482, #12314, #5111 ) ) ;
#843 = CARTESIAN_POINT ( 'NONE',  ( 11.54473802383823511, 36.35512261685320823, 55.24115706042309881 ) ) ;
#844 = DIRECTION ( 'NONE',  ( 0.000000000000000000, 0.000000000000000000, 1.000000000000000000 ) ) ;
#845 = DIRECTION ( 'NONE',  ( -1.000000000000000000, 0.000000000000000000, 0.000000000000000000 ) ) ;
#846 = DIRECTION ( 'NONE',  ( 0.000000000000000000, -0.000000000000000000, -1.000000000000000000 ) ) ;
#847 = AXIS2_PLACEMENT_3D ( 'NONE', #14671, #11121, #712 ) ;
#849 = ORIENTED_EDGE ( 'NONE', *, *, #20424, .F. ) ;
#848 = EDGE_CURVE ( 'NONE', #18961, #6724, #20651, .T. ) ;
#850 = ORIENTED_EDGE ( 'NONE', *, *, #1184, .T. ) ;
#851 = ORIENTED_EDGE ( 'NONE', *, *, #6390, .T. ) ;
#852 = ORIENTED_EDGE ( 'NONE', *, *, #561, .T. ) ;
#853 = CARTESIAN_POINT ( 'NONE',  ( 11.12045539253394821, 39.12082365973188303, 55.06303111140292827 ) ) ;
#854 = DIRECTION ( 'NONE',  ( 6.505213034913038160E-19, 3.903127820947822896E-18, 1.000000000000000000 ) ) ;
#855 = ADVANCED_FACE ( 'NONE', ( #10324, #6796 ), #5093, .F. ) ;
#856 = CARTESIAN_POINT ( 'NONE',  ( -17.00000000000002842, 20.00000000000000355, -102.0000000000000142 ) ) ;
#857 = ORIENTED_EDGE ( 'NONE', *, *, #19356, .F. ) ;
#858 = LINE ( 'NONE', #977, #13833 ) ;
#859 = DIRECTION ( 'NONE',  ( -1.000000000000000000, 0.000000000000000000, 0.000000000000000000 ) ) ;
#860 = ORIENTED_EDGE ( 'NONE', *, *, #4382, .T. ) ;
#861 = CIRCLE ( 'NONE', #8544, 2.499999999999995115 ) ;
#862 = VERTEX_POINT ( 'NONE', #13878 ) ;
#863 = DIRECTION ( 'NONE',  ( -6.505213034913038160E-19, -3.903127820947822896E-18, -1.000000000000000000 ) ) ;
#864 = CARTESIAN_POINT ( 'NONE',  ( -89.99999999999701572, -5.000000000000000000, -3.012171160963566127E-14 ) ) ;
#865 = DIRECTION ( 'NONE',  ( -0.000000000000000000, 1.000000000000000000, -0.000000000000000000 ) ) ;
#866 = CARTESIAN_POINT ( 'NONE',  ( -0.2719375495013811039, 39.99956352816811034, 48.94448636964621357 ) ) ;
#867 = TOROIDAL_SURFACE ( 'NONE', #1956, 50.00000000000000000, 10.00000000000000000 ) ;
#868 = VECTOR ( 'NONE', #22657, 1000.000000000000000 ) ;
#869 = CARTESIAN_POINT ( 'NONE',  ( -0.7060564148929356909, 40.00000000000297007, 49.41654780795607849 ) ) ;
#870 = CARTESIAN_POINT ( 'NONE',  ( 8.646032897229400049, -31.21605069118077580, -6.999999999999950262 ) ) ;
#871 = EDGE_CURVE ( 'NONE', #15231, #21079, #14775, .T. ) ;
#872 = ORIENTED_EDGE ( 'NONE', *, *, #16600, .F. ) ;
#873 = AXIS2_PLACEMENT_3D ( 'NONE', #3321, #3426, #13829 ) ;
#874 = ORIENTED_EDGE ( 'NONE', *, *, #14173, .F. ) ;
#875 = AXIS2_PLACEMENT_3D ( 'NONE', #12799, #6284, #13239 ) ;
#876 = VECTOR ( 'NONE', #4480, 1000.000000000000000 ) ;
#877 = VERTEX_POINT ( 'NONE', #17322 ) ;
#878 = CARTESIAN_POINT ( 'NONE',  ( -19.80158170751280977, 22.94611027470400089, 60.57464962002575959 ) ) ;
#879 = ADVANCED_FACE ( 'NONE', ( #8621, #20896 ), #5197, .F. ) ;
#880 = DIRECTION ( 'NONE',  ( 1.000000000000000000, 0.000000000000000000, 0.000000000000000000 ) ) ;
#881 = FACE_BOUND ( 'NONE', #13282, .T. ) ;
#882 = CARTESIAN_POINT ( 'NONE',  ( -0.3446551741029754701, -0.009348518860373671718, -50.24945914274646697 ) ) ;
#883 = CARTESIAN_POINT ( 'NONE',  ( -35.00000000000000000, 17.00000000000000000, -40.99999999999997868 ) ) ;
#884 = AXIS2_PLACEMENT_3D ( 'NONE', #22625, #19477, #2053 ) ;
#885 = DIRECTION ( 'NONE',  ( -1.000000000000000000, -1.208970125616063644E-17, 0.000000000000000000 ) ) ;
#886 = FACE_OUTER_BOUND ( 'NONE', #3171, .T. ) ;
#887 = CARTESIAN_POINT ( 'NONE',  ( -4.628075497661881421, 39.46063506869896997, -53.65703709786517805 ) ) ;
#888 = CARTESIAN_POINT ( 'NONE',  ( 34.00000000000000711, 28.19616000222403329, 4.163799117101000559E-15 ) ) ;
#889 = CARTESIAN_POINT ( 'NONE',  ( 35.00000000000058265, 40.00000000000000000, -52.90000000000076597 ) ) ;
#890 = CYLINDRICAL_SURFACE ( 'NONE', #9031, 1.000000000000000888 ) ;
#891 = PRODUCT ( 'CASE', 'CASE', '', ( #13512 ) ) ;
#892 = AXIS2_PLACEMENT_3D ( 'NONE', #18524, #18401, #17021 ) ;
#893 = EDGE_CURVE ( 'NONE', #11565, #12042, #19927, .T. ) ;
#894 = EDGE_LOOP ( 'NONE', ( #6024, #21589, #6688, #10460 ) ) ;
#895 = DIRECTION ( 'NONE',  ( 0.000000000000000000, 0.000000000000000000, -1.000000000000000000 ) ) ;
#896 = DIRECTION ( 'NONE',  ( 6.505213034913038160E-19, 3.903127820947822896E-18, 1.000000000000000000 ) ) ;
#897 = DIRECTION ( 'NONE',  ( 0.000000000000000000, 0.7071067811866457165, 0.7071067811864494290 ) ) ;
#898 = ORIENTED_EDGE ( 'NONE', *, *, #4527, .T. ) ;
#899 = CARTESIAN_POINT ( 'NONE',  ( 31.88709182564711142, -6.070730550691017413, 3.000000000000023537 ) ) ;
#900 = LINE ( 'NONE', #4353, #17009 ) ;
#901 = CARTESIAN_POINT ( 'NONE',  ( 13.83143812983114707, -29.36548507648029016, -7.000000000000006217 ) ) ;
#902 = CARTESIAN_POINT ( 'NONE',  ( 13.85640646055130709, -1.500000000000015099, -4.000000000000099476 ) ) ;
#903 = EDGE_CURVE ( 'NONE', #13935, #5360, #8572, .T. ) ;
#904 = EDGE_CURVE ( 'NONE', #353, #12856, #6012, .T. ) ;
#905 = CLOSED_SHELL ( 'NONE', ( #8563, #7076, #7929, #5678, #4465, #19150, #22576, #21458, #17712, #22222, #14782, #18419, #10391, #18239, #21785, #15928, #20178, #20226, #22233, #17927, #1863, #20395, #11837, #3599, #19443, #4692, #22628, #3299, #8649, #15514, #16721, #17259, #9019, #446, #1883, #17878, #8627, #15174, #20934, #10317, #17011, #430, #21730, #10433, #7354, #6426, #8274, #6528, #19882, #14280, #5310, #16856, #1353, #21124, #21999, #3977, #3481, #22065, #21190, #19028, #20680, #7463, #4335, #7078, #19523, #6625, #13775, #6600, #79, #8690, #20388, #3896, #2793, #13872, #15714, #5580, #19400, #10512, #8045, #12162, #18996, #15644, #12391, #11699, #344, #4559, #19376, #6148, #16346, #5545, #20631, #5202, #6959, #710, #4050, #13479, #14669, #14161, #1133, #2663, #18798, #4994, #14152, #14115, #16630, #13032, #3733, #10277, #7161, #2695, #3578, #1578, #655, #3354, #22650, #16686, #10847, #4861, #2677, #4727, #8678, #2175, #1764, #21366, #8230, #21822, #11023, #12771, #6554, #3602, #17130, #2598, #18208, #1841, #49, #6063, #16890, #12466, #17199, #15996, #21331, #8768, #2547, #8457, #22021, #6723, #20844, #21569, #17421, #5170, #16899, #4305, #11695, #22112, #22530, #9787, #17969, #8510, #5336, #13785, #10560, #17620, #13789, #1192, #21912, #3155, #19476, #2571, #13649, #2542, #11689, #2092, #18154, #9700, #18616, #5920, #14977, #20262, #5253, #5136, #6203, #12695, #20029, #16570, #21394, #16155, #16800, #21167, #16955, #6364, #9507, #16744, #8591, #19098, #1749, #6842, #21050, #6972, #17155, #19451, #8556 ) ) ;
#906 = ORIENTED_EDGE ( 'NONE', *, *, #22508, .T. ) ;
#907 = CARTESIAN_POINT ( 'NONE',  ( 34.74700806321121149, -12.00937115242670039, 2.800654218530512551 ) ) ;
#908 = EDGE_CURVE ( 'NONE', #19435, #14442, #4561, .T. ) ;
#909 = CARTESIAN_POINT ( 'NONE',  ( -4.025500340002513333, 36.54278193890309012, -2.800654218530457484 ) ) ;
#910 = ORIENTED_EDGE ( 'NONE', *, *, #12200, .F. ) ;
#911 = CARTESIAN_POINT ( 'NONE',  ( 0.5525046371098545350, 39.99819307499277699, -49.15917675262092246 ) ) ;
#912 = DIRECTION ( 'NONE',  ( 6.505213034913038160E-19, 3.903127820947822896E-18, 1.000000000000000000 ) ) ;
#913 = DIRECTION ( 'NONE',  ( 0.000000000000000000, 0.000000000000000000, 1.000000000000000000 ) ) ;
#914 = ADVANCED_FACE ( 'NONE', ( #16533 ), #19558, .F. ) ;
#915 = DIRECTION ( 'NONE',  ( -0.000000000000000000, 1.000000000000000000, -0.000000000000000000 ) ) ;
#916 = VECTOR ( 'NONE', #20039, 1000.000000000000000 ) ;
#917 = CARTESIAN_POINT ( 'NONE',  ( -15.97698236194133159, 7.938033795522204450, -59.50430813415450615 ) ) ;
#918 = DIRECTION ( 'NONE',  ( -1.000000000000000000, 0.000000000000000000, 0.000000000000000000 ) ) ;
#919 = AXIS2_PLACEMENT_3D ( 'NONE', #9251, #2386, #7658 ) ;
#920 = CARTESIAN_POINT ( 'NONE',  ( 17.38064605515585725, 30.98879172160187068, 3.000000000000048850 ) ) ;
#921 = EDGE_CURVE ( 'NONE', #10690, #11353, #1254, .T. ) ;
#922 = VERTEX_POINT ( 'NONE', #11605 ) ;
#923 = CARTESIAN_POINT ( 'NONE',  ( 35.00000000000058265, 26.00000000000000355, -55.00000000000076028 ) ) ;
#924 = CIRCLE ( 'NONE', #17694, 19.11328065563150957 ) ;
#925 = CYLINDRICAL_SURFACE ( 'NONE', #17707, 4.000000000000000000 ) ;
#926 = DIRECTION ( 'NONE',  ( -0.000000000000000000, -1.000000000000000000, -0.000000000000000000 ) ) ;
#927 = CIRCLE ( 'NONE', #18856, 2.099999999999997868 ) ;
#928 = VERTEX_POINT ( 'NONE', #1173 ) ;
#929 = CARTESIAN_POINT ( 'NONE',  ( -14.76055860720890500, 22.69766935715934153, 45.72055682016589628 ) ) ;
#930 = EDGE_CURVE ( 'NONE', #7391, #7282, #17354, .T. ) ;
#931 = CIRCLE ( 'NONE', #17391, 9.000000000000000000 ) ;
#933 = EDGE_CURVE ( 'NONE', #11968, #13427, #9674, .T. ) ;
#932 = ORIENTED_EDGE ( 'NONE', *, *, #1320, .T. ) ;
#934 = CIRCLE ( 'NONE', #6414, 36.76383501243555685 ) ;
#935 = B_SPLINE_CURVE_WITH_KNOTS ( 'NONE', 3,
 ( #21269, #3747, #5561, #17826, #19447, #174 ),
 .UNSPECIFIED., .F., .F.,
 ( 4, 2, 4 ),
 ( 1.991993874847888106E-18, 0.002694896630591175207, 0.005389793261182347812 ),
 .UNSPECIFIED. ) ;
#936 = ORIENTED_EDGE ( 'NONE', *, *, #12946, .T. ) ;
#937 = CARTESIAN_POINT ( 'NONE',  ( 153.1815963997936763, 176.5868022542937865, 33.35771513235977181 ) ) ;
#938 = VERTEX_POINT ( 'NONE', #20206 ) ;
#939 = CARTESIAN_POINT ( 'NONE',  ( 16.16780438139466014, 31.78273399965604540, 59.56292242448185448 ) ) ;
#940 = DIRECTION ( 'NONE',  ( 0.000000000000000000, 0.000000000000000000, -1.000000000000000000 ) ) ;
#941 = DIRECTION ( 'NONE',  ( 0.000000000000000000, 0.000000000000000000, 1.000000000000000000 ) ) ;
#942 = LINE ( 'NONE', #2210, #14631 ) ;
#943 = VERTEX_POINT ( 'NONE', #14908 ) ;
#944 = CARTESIAN_POINT ( 'NONE',  ( 34.99999999999999289, -5.000000000000000000, -54.99999999999705835 ) ) ;
#945 = CARTESIAN_POINT ( 'NONE',  ( 33.52953626616073279, 9.708269511265299911, -2.999999999999999112 ) ) ;
#946 = ORIENTED_EDGE ( 'NONE', *, *, #15805, .F. ) ;
#947 = CARTESIAN_POINT ( 'NONE',  ( -14.17374118098246605, 15.07546459525165261, -45.45638825402599537 ) ) ;
#948 = DIRECTION ( 'NONE',  ( 0.000000000000000000, 0.000000000000000000, -1.000000000000000000 ) ) ;
#949 = CARTESIAN_POINT ( 'NONE',  ( 16.97539716422056699, 9.395639044392945394, -59.81372721910505419 ) ) ;
#950 = VERTEX_POINT ( 'NONE', #9985 ) ;
#951 = CARTESIAN_POINT ( 'NONE',  ( -3.179547497537916545, 39.99999999999999289, -50.65098726527259743 ) ) ;
#952 = CARTESIAN_POINT ( 'NONE',  ( 0.3104238174410367535, 39.99820335227857271, -49.10409449009593175 ) ) ;
#953 = ORIENTED_EDGE ( 'NONE', *, *, #3177, .F. ) ;
#954 = CARTESIAN_POINT ( 'NONE',  ( -18.00000000000001421, 20.00000000000000711, 103.0000000000000284 ) ) ;
#955 = AXIS2_PLACEMENT_3D ( 'NONE', #2451, #833, #9435 ) ;
#956 = CARTESIAN_POINT ( 'NONE',  ( -21.05198877411806890, 30.13956425491229396, 2.800654218530481465 ) ) ;
#957 = AXIS2_PLACEMENT_3D ( 'NONE', #1200, #4989, #11969 ) ;
#958 = AXIS2_PLACEMENT_3D ( 'NONE', #6027, #9689, #16676 ) ;
#959 = ORIENTED_EDGE ( 'NONE', *, *, #1342, .F. ) ;
#960 = UNCERTAINTY_MEASURE_WITH_UNIT (LENGTH_MEASURE( 1.000000000000000082E-05 ), #19624, 'distance_accuracy_value', 'NONE');
#961 = CARTESIAN_POINT ( 'NONE',  ( 22.15900668633799597, 29.33526866242094755, 2.800654218530481465 ) ) ;
#962 = CARTESIAN_POINT ( 'NONE',  ( 2.775557561562891351E-14, 2.775557561562891351E-14, 5.750000000000001776 ) ) ;
#963 = CIRCLE ( 'NONE', #18169, 2.500000000000002220 ) ;
#964 = CARTESIAN_POINT ( 'NONE',  ( 19.96647043697146984, 18.54527240924682729, -60.61386395554088580 ) ) ;
#966 = ADVANCED_FACE ( 'NONE', ( #6228 ), #11858, .F. ) ;
#965 = ORIENTED_EDGE ( 'NONE', *, *, #15758, .T. ) ;
#967 = EDGE_LOOP ( 'NONE', ( #20857, #1137, #9405, #12556 ) ) ;
#968 = VERTEX_POINT ( 'NONE', #6113 ) ;
#969 = CIRCLE ( 'NONE', #14843, 1.000000000000000888 ) ;
#970 = VECTOR ( 'NONE', #5351, 1000.000000000000000 ) ;
#971 = CIRCLE ( 'NONE', #22574, 2.499999999999996891 ) ;
#972 = ORIENTED_EDGE ( 'NONE', *, *, #12220, .F. ) ;
#973 = CARTESIAN_POINT ( 'NONE',  ( 10.81645871535806336, 39.16817317914274810, 54.94897387137724110 ) ) ;
#974 = VECTOR ( 'NONE', #96, 1000.000000000000000 ) ;
#975 = EDGE_CURVE ( 'NONE', #10281, #6403, #8168, .T. ) ;
#976 = ORIENTED_EDGE ( 'NONE', *, *, #16314, .T. ) ;
#977 = CARTESIAN_POINT ( 'NONE',  ( -33.51030287062356194, -15.12081897056691204, -2.000000000000005329 ) ) ;
#978 = CARTESIAN_POINT ( 'NONE',  ( -2.615521992622583891, 14.48472893833976016, 6.613019222488492943 ) ) ;
#979 = ORIENTED_EDGE ( 'NONE', *, *, #10273, .F. ) ;
#980 = DIRECTION ( 'NONE',  ( -6.505213034913038160E-19, -3.903127820947822896E-18, -1.000000000000000000 ) ) ;
#981 = AXIS2_PLACEMENT_3D ( 'NONE', #21390, #5359, #15768 ) ;
#982 = EDGE_LOOP ( 'NONE', ( #22438, #1446 ) ) ;
#983 = CARTESIAN_POINT ( 'NONE',  ( -1.485717122675833668, -1.299971956346735791, -49.29290837556842320 ) ) ;
#984 = DIRECTION ( 'NONE',  ( 0.000000000000000000, 0.000000000000000000, -1.000000000000000000 ) ) ;
#985 = CARTESIAN_POINT ( 'NONE',  ( 0.000000000000000000, 9.999999999999998224, 0.000000000000000000 ) ) ;
#986 = CARTESIAN_POINT ( 'NONE',  ( -35.91964150878168027, -4.104665049622911788, -2.933296326616361416 ) ) ;
#987 = ADVANCED_FACE ( 'NONE', ( #11375 ), #158, .F. ) ;
#988 = CARTESIAN_POINT ( 'NONE',  ( 1.734786545154649763E-13, 1.500000000000004885, -16.00000000000029488 ) ) ;
#989 = CYLINDRICAL_SURFACE ( 'NONE', #17809, 16.49999999999998579 ) ;
#990 = EDGE_LOOP ( 'NONE', ( #5095, #11437, #19565, #9961 ) ) ;
#991 = VECTOR ( 'NONE', #14455, 1000.000000000000000 ) ;
#992 = ORIENTED_EDGE ( 'NONE', *, *, #14848, .T. ) ;
#993 = ORIENTED_EDGE ( 'NONE', *, *, #18740, .F. ) ;
#994 = CARTESIAN_POINT ( 'NONE',  ( -20.65262896361484835, 28.82759387226903769, 58.26038807538093778 ) ) ;
#995 = FACE_OUTER_BOUND ( 'NONE', #22560, .T. ) ;
#996 = AXIS2_PLACEMENT_3D ( 'NONE', #6782, #6667, #13523 ) ;
#997 = CARTESIAN_POINT ( 'NONE',  ( -34.99999999999999289, 0.000000000000000000, -58.99999999999701572 ) ) ;
#998 = CARTESIAN_POINT ( 'NONE',  ( -11.45074849662542782, 39.99999999999999289, 54.12667998692793958 ) ) ;
#999 = DIRECTION ( 'NONE',  ( 0.000000000000000000, 0.000000000000000000, 1.000000000000000000 ) ) ;
#1000 = CARTESIAN_POINT ( 'NONE',  ( -90.00000000000000000, 40.00000000000000711, -2.525000000000000355 ) ) ;
#1001 = CARTESIAN_POINT ( 'NONE',  ( 3.210598435713497345, 39.75302854575188150, 52.30739040051271616 ) ) ;
#1002 = DIRECTION ( 'NONE',  ( 1.000000000000000000, 1.208970125616053475E-17, 0.000000000000000000 ) ) ;
#1003 = CARTESIAN_POINT ( 'NONE',  ( -2.568452277497750937E-14, 40.00000000000000000, -48.73397172404482092 ) ) ;
#1004 = ADVANCED_FACE ( 'NONE', ( #2680 ), #15298, .T. ) ;
#1005 = EDGE_LOOP ( 'NONE', ( #5740, #22368, #2661, #14334 ) ) ;
#1006 = CIRCLE ( 'NONE', #13433, 39.00000000000000000 ) ;
#1007 = AXIS2_PLACEMENT_3D ( 'NONE', #13919, #17486, #21158 ) ;
#1008 = DIRECTION ( 'NONE',  ( 0.000000000000000000, 1.000000000000000000, 0.000000000000000000 ) ) ;
#1009 = CARTESIAN_POINT ( 'NONE',  ( 42.49999999999998579, 7.000000000000000000, -49.99999999999997868 ) ) ;
#1010 = DIRECTION ( 'NONE',  ( 1.000000000000000000, 1.208970125616053321E-17, 0.000000000000000000 ) ) ;
#1011 = CARTESIAN_POINT ( 'NONE',  ( 35.00000000000001421, -5.000000000000000000, 1.540743955509788682E-30 ) ) ;
#1012 = EDGE_CURVE ( 'NONE', #17260, #11580, #15474, .T. ) ;
#1013 = ORIENTED_EDGE ( 'NONE', *, *, #6207, .T. ) ;
#1014 = AXIS2_PLACEMENT_3D ( 'NONE', #14105, #8524, #15499 ) ;
#1015 = ORIENTED_EDGE ( 'NONE', *, *, #2081, .T. ) ;
#1016 = CARTESIAN_POINT ( 'NONE',  ( -42.50000000000000711, -11.97499999999999964, -45.00000000000000000 ) ) ;
#1017 = DIRECTION ( 'NONE',  ( -0.000000000000000000, 1.000000000000000000, -0.000000000000000000 ) ) ;
#1018 = AXIS2_PLACEMENT_3D ( 'NONE', #22227, #12123, #15545 ) ;
#1019 = CARTESIAN_POINT ( 'NONE',  ( 37.07861450834818129, -3.656418565264468512, -6.999999999999999112 ) ) ;
#1020 = EDGE_CURVE ( 'NONE', #18887, #21019, #14081, .T. ) ;
#1021 = AXIS2_PLACEMENT_3D ( 'NONE', #20944, #11063, #530 ) ;
#1022 = DIRECTION ( 'NONE',  ( 6.505213034913038160E-19, 3.903127820947822896E-18, 1.000000000000000000 ) ) ;
#1023 = ORIENTED_EDGE ( 'NONE', *, *, #11379, .T. ) ;
#1024 = CARTESIAN_POINT ( 'NONE',  ( 3.072145818613496449, 39.94358020626381744, -50.97359800879427638 ) ) ;
#1025 = CIRCLE ( 'NONE', #15655, 31.50000000000001421 ) ;
#1026 = CIRCLE ( 'NONE', #652, 2.500000000000002220 ) ;
#1027 = DIRECTION ( 'NONE',  ( 0.000000000000000000, -1.000000000000000000, 0.000000000000000000 ) ) ;
#1028 = VECTOR ( 'NONE', #21615, 1000.000000000000000 ) ;
#1029 = DIRECTION ( 'NONE',  ( -1.000000000000000000, -1.208970125616060717E-17, 0.000000000000000000 ) ) ;
#1030 = CARTESIAN_POINT ( 'NONE',  ( -5.004759427256008308, 40.00000000000000000, 51.61237555825404399 ) ) ;
#1031 = ADVANCED_FACE ( 'NONE', ( #10212 ), #3584, .T. ) ;
#1032 = CARTESIAN_POINT ( 'NONE',  ( 35.00000000000000000, 0.000000000000000000, -40.99999999999997868 ) ) ;
#1033 = AXIS2_PLACEMENT_3D ( 'NONE', #8268, #15697, #15237 ) ;
#1034 = DIRECTION ( 'NONE',  ( -1.000000000000000000, -1.208970125616077665E-17, 0.000000000000000000 ) ) ;
#1035 = DIRECTION ( 'NONE',  ( 5.292376706370188309E-15, 0.000000000000000000, 1.000000000000000000 ) ) ;
#1036 = EDGE_LOOP ( 'NONE', ( #13313, #7843, #1348, #16196 ) ) ;
#1037 = CARTESIAN_POINT ( 'NONE',  ( 14.04383866228953792, 25.28361825225916704, 45.39674436955350956 ) ) ;
#1038 = DIRECTION ( 'NONE',  ( 0.000000000000000000, 0.000000000000000000, -1.000000000000000000 ) ) ;
#1039 = FACE_OUTER_BOUND ( 'NONE', #8515, .T. ) ;
#1040 = CARTESIAN_POINT ( 'NONE',  ( 12.99999999999993960, 42.51666049839543149, 60.00099999999999767 ) ) ;
#1041 = B_SPLINE_CURVE_WITH_KNOTS ( 'NONE', 3,
 ( #15282, #19394, #22410, #15505 ),
 .UNSPECIFIED., .F., .F.,
 ( 4, 4 ),
 ( 0.001893031756885169004, 0.003808480026563660498 ),
 .UNSPECIFIED. ) ;
#1042 = DIRECTION ( 'NONE',  ( -0.000000000000000000, -0.000000000000000000, -1.000000000000000000 ) ) ;
#1043 = EDGE_LOOP ( 'NONE', ( #3805, #13880, #14516, #5311 ) ) ;
#1044 = AXIS2_PLACEMENT_3D ( 'NONE', #4036, #2841, #6275 ) ;
#1045 = CARTESIAN_POINT ( 'NONE',  ( -14.05436202270911217, 25.29714423467776996, 45.40204559108968141 ) ) ;
#1046 = DIRECTION ( 'NONE',  ( 6.505213034913038160E-19, 3.903127820947822896E-18, 1.000000000000000000 ) ) ;
#1047 = AXIS2_PLACEMENT_3D ( 'NONE', #633, #15979, #290 ) ;
#1048 = AXIS2_PLACEMENT_3D ( 'NONE', #20032, #4338, #1002 ) ;
#1049 = CIRCLE ( 'NONE', #8360, 2.499999999999998668 ) ;
#1050 = ORIENTED_EDGE ( 'NONE', *, *, #320, .T. ) ;
#1051 = EDGE_CURVE ( 'NONE', #1297, #18279, #13311, .T. ) ;
#1052 = ORIENTED_EDGE ( 'NONE', *, *, #13195, .T. ) ;
#1053 = CARTESIAN_POINT ( 'NONE',  ( 188.3927799473842697, 176.4612793482023676, -25.51636063260277965 ) ) ;
#1054 = VERTEX_POINT ( 'NONE', #20767 ) ;
#1055 = CARTESIAN_POINT ( 'NONE',  ( 14.31751149541521784, 33.97259629115305302, -58.93694582298954998 ) ) ;
#1056 = CARTESIAN_POINT ( 'NONE',  ( 0.000000000000000000, -40.00000000000000000, 0.000000000000000000 ) ) ;
#1057 = CARTESIAN_POINT ( 'NONE',  ( 0.003185071962414435728, 24.99999830921895594, 8.999999436406460163 ) ) ;
#1058 = CARTESIAN_POINT ( 'NONE',  ( -34.99999999999999289, 0.000000000000000000, 50.00000000000000000 ) ) ;
#1059 = VECTOR ( 'NONE', #10373, 1000.000000000000000 ) ;
#1060 = CARTESIAN_POINT ( 'NONE',  ( -5.074925817841801745, 32.10132595304121850, -6.999999999999950262 ) ) ;
#1061 = ORIENTED_EDGE ( 'NONE', *, *, #730, .T. ) ;
#1062 = DIRECTION ( 'NONE',  ( -0.000000000000000000, -1.000000000000000000, -0.000000000000000000 ) ) ;
#1064 = CIRCLE ( 'NONE', #7639, 36.76383501243555685 ) ;
#1063 = DIRECTION ( 'NONE',  ( 0.000000000000000000, 0.7071067811865549002, 0.7071067811865402453 ) ) ;
#1065 = ORIENTED_EDGE ( 'NONE', *, *, #16608, .T. ) ;
#1066 = EDGE_CURVE ( 'NONE', #22056, #12221, #10745, .T. ) ;
#1067 = EDGE_CURVE ( 'NONE', #17407, #7645, #438, .T. ) ;
#1068 = DIRECTION ( 'NONE',  ( 1.000000000000000000, 0.000000000000000000, 0.000000000000000000 ) ) ;
#1069 = EDGE_CURVE ( 'NONE', #407, #1418, #13674, .T. ) ;
#1070 = LINE ( 'NONE', #609, #17776 ) ;
#1071 = FACE_OUTER_BOUND ( 'NONE', #3229, .T. ) ;
#1072 = CARTESIAN_POINT ( 'NONE',  ( 29.36548507648026174, 13.83143812983086995, 3.000000000000023537 ) ) ;
#1073 = ORIENTED_EDGE ( 'NONE', *, *, #4590, .T. ) ;
#1074 = CARTESIAN_POINT ( 'NONE',  ( -5.234365469061698306, 40.00000000000000711, -51.72901482534432205 ) ) ;
#1075 = CARTESIAN_POINT ( 'NONE',  ( 8.331955809010596070, 38.18181818181818699, -56.36098470834070895 ) ) ;
#1076 = ORIENTED_EDGE ( 'NONE', *, *, #6843, .F. ) ;
#1077 = CARTESIAN_POINT ( 'NONE',  ( 9.375581681113587251, 39.53990230686088836, 54.37755644423855017 ) ) ;
#1078 = FACE_OUTER_BOUND ( 'NONE', #20598, .T. ) ;
#1079 = CARTESIAN_POINT ( 'NONE',  ( -2.951413581184478829, -1.204958657596112870, -50.23354289400218420 ) ) ;
#1080 = EDGE_LOOP ( 'NONE', ( #4988, #8993, #12256, #12165, #18775, #10133 ) ) ;
#1081 = DIRECTION ( 'NONE',  ( -1.000000000000000000, -1.208970125616081209E-17, 0.000000000000000000 ) ) ;
#1082 = EDGE_CURVE ( 'NONE', #8936, #13925, #9174, .T. ) ;
#1083 = CARTESIAN_POINT ( 'NONE',  ( -15.00000000000001421, 20.00000000000000000, -101.0000000000000284 ) ) ;
#1084 = CARTESIAN_POINT ( 'NONE',  ( 19.64963058618602787, 23.83053889023033634, -60.53829769526750937 ) ) ;
#1085 = AXIS2_PLACEMENT_3D ( 'NONE', #4347, #671, #12905 ) ;
#1086 = ORIENTED_EDGE ( 'NONE', *, *, #5522, .F. ) ;
#1087 = ORIENTED_EDGE ( 'NONE', *, *, #13548, .F. ) ;
#1088 = VERTEX_POINT ( 'NONE', #16387 ) ;
#1089 = VERTEX_POINT ( 'NONE', #12592 ) ;
#1090 = CARTESIAN_POINT ( 'NONE',  ( 11.25639079644659724, 39.09917355294047780, 55.11545576760340026 ) ) ;
#1091 = CARTESIAN_POINT ( 'NONE',  ( -28.52469787935782364, 7.000000000000000000, 4.095854054471899985 ) ) ;
#1092 = ORIENTED_EDGE ( 'NONE', *, *, #11379, .F. ) ;
#1093 = DIRECTION ( 'NONE',  ( 6.505213034913038160E-19, 3.903127820947822896E-18, 1.000000000000000000 ) ) ;
#1094 = CARTESIAN_POINT ( 'NONE',  ( -0.3961047786457937980, 13.02071089460816822, 6.993377406885125325 ) ) ;
#1095 = ORIENTED_EDGE ( 'NONE', *, *, #6767, .T. ) ;
#1096 = DIRECTION ( 'NONE',  ( 0.000000000000000000, 0.000000000000000000, -1.000000000000000000 ) ) ;
#1097 = CARTESIAN_POINT ( 'NONE',  ( 12.09218358684717920, 1.291952833853752924, 55.42846997241154838 ) ) ;
#1098 = AXIS2_PLACEMENT_3D ( 'NONE', #16217, #413, #16338 ) ;
#1099 = ORIENTED_EDGE ( 'NONE', *, *, #9484, .F. ) ;
#1100 = DIRECTION ( 'NONE',  ( 0.000000000000000000, 0.000000000000000000, 1.000000000000000000 ) ) ;
#1101 = DIRECTION ( 'NONE',  ( -0.000000000000000000, -1.000000000000000000, -0.000000000000000000 ) ) ;
#1102 = CARTESIAN_POINT ( 'NONE',  ( -18.50805780747144880, 27.59542556733953944, -60.24679276096814817 ) ) ;
#1103 = EDGE_CURVE ( 'NONE', #4270, #21371, #16147, .T. ) ;
#1104 = EDGE_CURVE ( 'NONE', #14723, #11771, #19837, .T. ) ;
#1105 = AXIS2_PLACEMENT_3D ( 'NONE', #8719, #1616, #8487 ) ;
#1106 = CARTESIAN_POINT ( 'NONE',  ( 10.30713387248687773, 2.842164160680653584, -57.27491564205610786 ) ) ;
#1107 = ADVANCED_FACE ( 'NONE', ( #21321 ), #701, .F. ) ;
#1108 = ORIENTED_EDGE ( 'NONE', *, *, #189, .F. ) ;
#1109 = EDGE_LOOP ( 'NONE', ( #375, #3783, #3352, #21228, #19143, #12835 ) ) ;
#1110 = CIRCLE ( 'NONE', #20504, 1.000000000000000888 ) ;
#1111 = ORIENTED_EDGE ( 'NONE', *, *, #17841, .F. ) ;
#1112 = CARTESIAN_POINT ( 'NONE',  ( -19.96647043697144852, 18.54527240924516818, 60.61386395554428219 ) ) ;
#1113 = DIRECTION ( 'NONE',  ( -1.000000000000000000, 0.000000000000000000, 0.000000000000000000 ) ) ;
#1114 = DIRECTION ( 'NONE',  ( 6.505213034913038160E-19, 3.903127820947822896E-18, 1.000000000000000000 ) ) ;
#1115 = CARTESIAN_POINT ( 'NONE',  ( -11.28246622563948520, 40.00000000000000711, 54.06713842414183802 ) ) ;
#1116 = AXIS2_PLACEMENT_3D ( 'NONE', #1709, #13712, #16941 ) ;
#1117 = ORIENTED_EDGE ( 'NONE', *, *, #4115, .T. ) ;
#1118 = DIRECTION ( 'NONE',  ( -1.000000000000000000, 0.000000000000000000, 0.000000000000000000 ) ) ;
#1119 = CARTESIAN_POINT ( 'NONE',  ( -34.99999999999980815, 40.00000000000000000, 54.99999999999922551 ) ) ;
#1120 = FACE_OUTER_BOUND ( 'NONE', #7332, .T. ) ;
#1121 = CARTESIAN_POINT ( 'NONE',  ( -5.133444049470117676, 39.34078687931064167, -53.02546735988109816 ) ) ;
#1122 = DIRECTION ( 'NONE',  ( 0.000000000000000000, 0.000000000000000000, 1.000000000000000000 ) ) ;
#1123 = ORIENTED_EDGE ( 'NONE', *, *, #11097, .F. ) ;
#1124 = DIRECTION ( 'NONE',  ( -0.000000000000000000, 1.000000000000000000, -0.000000000000000000 ) ) ;
#1125 = DIRECTION ( 'NONE',  ( 0.000000000000000000, 0.000000000000000000, -1.000000000000000000 ) ) ;
#1126 = DIRECTION ( 'NONE',  ( 0.000000000000000000, -0.000000000000000000, -1.000000000000000000 ) ) ;
#1127 = EDGE_LOOP ( 'NONE', ( #10984, #4974, #21316, #12105 ) ) ;
#1128 = DIRECTION ( 'NONE',  ( -6.505213034913038160E-19, -3.903127820947822896E-18, -1.000000000000000000 ) ) ;
#1129 = CARTESIAN_POINT ( 'NONE',  ( 31.41239365194228839, -2.347663744114464102, -2.999999999999999112 ) ) ;
#1130 = CARTESIAN_POINT ( 'NONE',  ( 34.64233806479157352, 10.34893680499398272, 2.932969818539056472 ) ) ;
#1131 = EDGE_LOOP ( 'NONE', ( #16120, #1991 ) ) ;
#1132 = AXIS2_PLACEMENT_3D ( 'NONE', #8155, #6437, #14895 ) ;
#1133 = ADVANCED_FACE ( 'NONE', ( #15921 ), #5617, .F. ) ;
#1134 = ORIENTED_EDGE ( 'NONE', *, *, #7502, .T. ) ;
#1135 = CARTESIAN_POINT ( 'NONE',  ( -4.044995508448087307, -4.680814751541408469, 48.25214090642531772 ) ) ;
#1136 = DIRECTION ( 'NONE',  ( -0.000000000000000000, -1.000000000000000000, -0.000000000000000000 ) ) ;
#1137 = ORIENTED_EDGE ( 'NONE', *, *, #19566, .F. ) ;
#1138 = EDGE_CURVE ( 'NONE', #16070, #18599, #7758, .T. ) ;
#1139 = DIRECTION ( 'NONE',  ( 1.000000000000000000, 0.000000000000000000, 0.000000000000000000 ) ) ;
#1140 = DIRECTION ( 'NONE',  ( 1.000000000000000000, 0.000000000000000000, 0.000000000000000000 ) ) ;
#1141 = CARTESIAN_POINT ( 'NONE',  ( 5.551115123125782702E-14, -1.387778780781445676E-13, -5.749999999999949374 ) ) ;
#1142 = CARTESIAN_POINT ( 'NONE',  ( 10.77132920883424205, 39.17511451497404806, -54.93228420922696387 ) ) ;
#1143 = FACE_OUTER_BOUND ( 'NONE', #9305, .T. ) ;
#1144 = FACE_OUTER_BOUND ( 'NONE', #11608, .T. ) ;
#1145 = ORIENTED_EDGE ( 'NONE', *, *, #20842, .T. ) ;
#1146 = LINE ( 'NONE', #22009, #3920 ) ;
#1147 = CARTESIAN_POINT ( 'NONE',  ( 6.041077103367500811, -0.8288449397161629095, 52.13906252460464685 ) ) ;
#1148 = CARTESIAN_POINT ( 'NONE',  ( 8.219889501001356180, 1.750964516533152437, -56.08920281153656617 ) ) ;
#1149 = CARTESIAN_POINT ( 'NONE',  ( -1.387778780781445676E-14, 40.00000000000000000, -48.73397172404481381 ) ) ;
#1150 = VERTEX_POINT ( 'NONE', #19494 ) ;
#1151 = EDGE_CURVE ( 'NONE', #1471, #10193, #15429, .T. ) ;
#1152 = CARTESIAN_POINT ( 'NONE',  ( 2.775557561562891351E-14, 2.775557561562891351E-14, 5.750000000000001776 ) ) ;
#1153 = DIRECTION ( 'NONE',  ( 0.000000000000000000, 1.000000000000000000, 0.000000000000000000 ) ) ;
#1154 = CIRCLE ( 'NONE', #13936, 19.11328065563152023 ) ;
#1155 = EDGE_CURVE ( 'NONE', #18643, #19011, #9589, .T. ) ;
#1156 = ORIENTED_EDGE ( 'NONE', *, *, #12333, .T. ) ;
#1157 = VERTEX_POINT ( 'NONE', #459 ) ;
#1158 = EDGE_LOOP ( 'NONE', ( #1280, #14441, #11642, #13027 ) ) ;
#1159 = CARTESIAN_POINT ( 'NONE',  ( 19.41351212956690730, 24.83257706694782030, -60.47995209899215041 ) ) ;
#1160 = ADVANCED_FACE ( 'NONE', ( #14426 ), #18742, .T. ) ;
#1161 = CARTESIAN_POINT ( 'NONE',  ( 5.833333333333336590, 39.00000000000000711, 40.61164310337068173 ) ) ;
#1162 = DIRECTION ( 'NONE',  ( 1.000000000000000000, 0.000000000000000000, 0.000000000000000000 ) ) ;
#1163 = DIRECTION ( 'NONE',  ( 0.000000000000000000, 0.000000000000000000, 1.000000000000000000 ) ) ;
#1164 = CARTESIAN_POINT ( 'NONE',  ( 0.5279010140432808251, 4.999719073153301885, -38.73355033370100386 ) ) ;
#1165 = ORIENTED_EDGE ( 'NONE', *, *, #11487, .F. ) ;
#1166 = DIRECTION ( 'NONE',  ( -1.000000000000000000, 0.000000000000000000, 0.000000000000000000 ) ) ;
#1167 = LINE ( 'NONE', #8160, #14153 ) ;
#1168 = ORIENTED_EDGE ( 'NONE', *, *, #20660, .T. ) ;
#1169 = CARTESIAN_POINT ( 'NONE',  ( -31.11359284679382498, -4.918774254216079278, -2.999999999999971578 ) ) ;
#1170 = DIRECTION ( 'NONE',  ( -1.000000000000000000, 0.000000000000000000, 0.000000000000000000 ) ) ;
#1171 = LINE ( 'NONE', #6331, #5023 ) ;
#1172 = ORIENTED_EDGE ( 'NONE', *, *, #2942, .F. ) ;
#1173 = CARTESIAN_POINT ( 'NONE',  ( -34.24928931925748543, 6.742883674876520850, -2.999999999999957367 ) ) ;
#1174 = CARTESIAN_POINT ( 'NONE',  ( -1.387778780781445676E-14, 40.00000000000000000, -48.73397172404481381 ) ) ;
#1175 = ORIENTED_EDGE ( 'NONE', *, *, #2779, .F. ) ;
#1176 = LINE ( 'NONE', #13633, #12302 ) ;
#1177 = EDGE_LOOP ( 'NONE', ( #4533, #4568 ) ) ;
#1178 = DIRECTION ( 'NONE',  ( -6.505213034913038160E-19, -3.903127820947822896E-18, -1.000000000000000000 ) ) ;
#1179 = EDGE_CURVE ( 'NONE', #14813, #15106, #21665, .T. ) ;
#1180 = DIRECTION ( 'NONE',  ( 0.000000000000000000, 1.000000000000000000, 0.000000000000000000 ) ) ;
#1181 = DIRECTION ( 'NONE',  ( -0.000000000000000000, -0.000000000000000000, 1.000000000000000000 ) ) ;
#1182 = CARTESIAN_POINT ( 'NONE',  ( 17.96966555604127791, 28.82469637350566671, -60.10139901455266198 ) ) ;
#1183 = EDGE_CURVE ( 'NONE', #15016, #19404, #7569, .T. ) ;
#1184 = EDGE_CURVE ( 'NONE', #18333, #16148, #3013, .T. ) ;
#1185 = ORIENTED_EDGE ( 'NONE', *, *, #5813, .F. ) ;
#1186 = AXIS2_PLACEMENT_3D ( 'NONE', #12099, #19093, #17360 ) ;
#1187 = VERTEX_POINT ( 'NONE', #10645 ) ;
#1188 = EDGE_LOOP ( 'NONE', ( #4686, #20113, #19205, #17754, #20799, #14313 ) ) ;
#1189 = ORIENTED_EDGE ( 'NONE', *, *, #16482, .F. ) ;
#1190 = CARTESIAN_POINT ( 'NONE',  ( 10.87562399044275274, 39.15903841214502279, 54.97094722865957550 ) ) ;
#1191 = DIRECTION ( 'NONE',  ( -0.1421319796954317316, 0.000000000000000000, -0.9898477157360405787 ) ) ;
#1192 = ADVANCED_FACE ( 'NONE', ( #236 ), #10760, .T. ) ;
#1193 = ORIENTED_EDGE ( 'NONE', *, *, #10418, .F. ) ;
#1194 = CYLINDRICAL_SURFACE ( 'NONE', #10169, 19.11328065563151668 ) ;
#1195 = CARTESIAN_POINT ( 'NONE',  ( -4.842578813368415780, -0.8535550256952800785, -51.47191290771856131 ) ) ;
#1196 = ORIENTED_EDGE ( 'NONE', *, *, #19405, .T. ) ;
#1197 = DIRECTION ( 'NONE',  ( 0.000000000000000000, 0.000000000000000000, 1.000000000000000000 ) ) ;
#1198 = CARTESIAN_POINT ( 'NONE',  ( 9.857944917837743404, 0.2919354798308393395, 54.29891737064654222 ) ) ;
#1199 = ORIENTED_EDGE ( 'NONE', *, *, #1318, .F. ) ;
#1200 = CARTESIAN_POINT ( 'NONE',  ( 35.00000000000058265, 40.00000000000000000, -55.00000000000076028 ) ) ;
#1201 = ADVANCED_FACE ( 'NONE', ( #7344 ), #11115, .F. ) ;
#1202 = DIRECTION ( 'NONE',  ( 0.000000000000000000, 0.000000000000000000, -1.000000000000000000 ) ) ;
#1203 = DIRECTION ( 'NONE',  ( -0.000000000000000000, -0.000000000000000000, -1.000000000000000000 ) ) ;
#1204 = CARTESIAN_POINT ( 'NONE',  ( -12.24033418603700873, 35.84417766536505923, -58.14550894043696161 ) ) ;
#1205 = AXIS2_PLACEMENT_3D ( 'NONE', #2980, #20505, #19016 ) ;
#1206 = EDGE_CURVE ( 'NONE', #14456, #5141, #2188, .T. ) ;
#1207 = CARTESIAN_POINT ( 'NONE',  ( -14.92530643917655375, 18.45549920837825653, 45.79309713780078539 ) ) ;
#1208 = ORIENTED_EDGE ( 'NONE', *, *, #15769, .F. ) ;
#1209 = ORIENTED_EDGE ( 'NONE', *, *, #1765, .F. ) ;
#1210 = ADVANCED_FACE ( 'NONE', ( #5858 ), #7792, .F. ) ;
#1211 = ORIENTED_EDGE ( 'NONE', *, *, #10301, .T. ) ;
#1212 = CARTESIAN_POINT ( 'NONE',  ( -18.15458487487865114, 6.756534690977250790, 57.58998093367232940 ) ) ;
#1213 = LINE ( 'NONE', #6269, #13676 ) ;
#1214 = VECTOR ( 'NONE', #15855, 1000.000000000000000 ) ;
#1215 = VECTOR ( 'NONE', #22012, 1000.000000000000000 ) ;
#1216 = CARTESIAN_POINT ( 'NONE',  ( -19.23800698326016700, 14.47374112874266316, -60.43633296823762890 ) ) ;
#1217 = CARTESIAN_POINT ( 'NONE',  ( 9.075375594263590528, 39.43595020987488198, 54.33405310157220924 ) ) ;
#1218 = AXIS2_PLACEMENT_3D ( 'NONE', #16052, #4046, #11014 ) ;
#1219 = FACE_OUTER_BOUND ( 'NONE', #18138, .T. ) ;
#1220 = EDGE_LOOP ( 'NONE', ( #16663, #20723, #12377, #11901, #7553, #4761 ) ) ;
#1221 = CARTESIAN_POINT ( 'NONE',  ( 41.39271818392636959, 7.000000000000000000, -5.943569790512535533 ) ) ;
#1222 = CARTESIAN_POINT ( 'NONE',  ( -13.00000000000011546, 42.51666049839536043, 105.0000000000000142 ) ) ;
#1223 = CARTESIAN_POINT ( 'NONE',  ( -0.5687583343899673682, -4.666323447581315342, 48.32169744526331812 ) ) ;
#1224 = CARTESIAN_POINT ( 'NONE',  ( 19.59430950039317665, -28.88846368933348074, -2.999999999999999112 ) ) ;
#1225 = ORIENTED_EDGE ( 'NONE', *, *, #15054, .T. ) ;
#1226 = AXIS2_PLACEMENT_3D ( 'NONE', #17024, #22324, #13460 ) ;
#1227 = CARTESIAN_POINT ( 'NONE',  ( -10.07716038413160220, 39.27871711242732289, 54.68297691402418792 ) ) ;
#1228 = FACE_OUTER_BOUND ( 'NONE', #10168, .T. ) ;
#1229 = ORIENTED_EDGE ( 'NONE', *, *, #6730, .F. ) ;
#1230 = VECTOR ( 'NONE', #854, 1000.000000000000000 ) ;
#1231 = CARTESIAN_POINT ( 'NONE',  ( 4.929203366568097207E-16, 30.00000000000000355, -4.025000000000000355 ) ) ;
#1232 = CARTESIAN_POINT ( 'NONE',  ( -34.99999999999980815, 40.00000000000000000, 54.99999999999922551 ) ) ;
#1233 = FACE_BOUND ( 'NONE', #5891, .T. ) ;
#1234 = AXIS2_PLACEMENT_3D ( 'NONE', #18228, #14666, #5966 ) ;
#1235 = VECTOR ( 'NONE', #4378, 1000.000000000000000 ) ;
#1236 = ORIENTED_EDGE ( 'NONE', *, *, #4757, .T. ) ;
#1237 = EDGE_CURVE ( 'NONE', #21534, #5255, #14095, .T. ) ;
#1238 = ORIENTED_EDGE ( 'NONE', *, *, #7866, .T. ) ;
#1239 = CARTESIAN_POINT ( 'NONE',  ( -34.99999999999980815, 40.00000000000000711, 54.99999999999922551 ) ) ;
#1240 = AXIS2_PLACEMENT_3D ( 'NONE', #16313, #6008, #623 ) ;
#1241 = DIRECTION ( 'NONE',  ( 0.000000000000000000, 0.000000000000000000, 1.000000000000000000 ) ) ;
#1242 = EDGE_LOOP ( 'NONE', ( #6996, #21007, #22630, #22192 ) ) ;
#1243 = CARTESIAN_POINT ( 'NONE',  ( -14.93538271375417814, -34.13396246814587442, -6.999999999999950262 ) ) ;
#1244 = TOROIDAL_SURFACE ( 'NONE', #873, 34.90673715956759082, 8.750000000000000000 ) ;
#1245 = EDGE_CURVE ( 'NONE', #4801, #14603, #15791, .T. ) ;
#1246 = FACE_OUTER_BOUND ( 'NONE', #2056, .T. ) ;
#1247 = CARTESIAN_POINT ( 'NONE',  ( 89.99999999999701572, 0.000000000000000000, -2.500000000000060840 ) ) ;
#1248 = CARTESIAN_POINT ( 'NONE',  ( -19.67353980729183860, 23.69994786803828646, -58.06093965453396066 ) ) ;
#1249 = AXIS2_PLACEMENT_3D ( 'NONE', #16047, #355, #4140 ) ;
#1250 = CARTESIAN_POINT ( 'NONE',  ( -8.115799706357579524, 39.55796121550449129, 53.89994064586117872 ) ) ;
#1251 = DIRECTION ( 'NONE',  ( -6.505213034913038160E-19, -3.903127820947822896E-18, -1.000000000000000000 ) ) ;
#1252 = ORIENTED_EDGE ( 'NONE', *, *, #21699, .F. ) ;
#1253 = CARTESIAN_POINT ( 'NONE',  ( 11.13407802442741357, 30.05807871779230922, 43.93745127716450583 ) ) ;
#1254 = B_SPLINE_CURVE_WITH_KNOTS ( 'NONE', 3,
 ( #836, #7825, #22270, #16763 ),
 .UNSPECIFIED., .F., .F.,
 ( 4, 4 ),
 ( 9.715086431488502079E-07, 0.001929643240674611517 ),
 .UNSPECIFIED. ) ;
#1255 = DIRECTION ( 'NONE',  ( 1.000000000000000000, 1.208970125616062874E-17, 0.000000000000000000 ) ) ;
#1256 = CARTESIAN_POINT ( 'NONE',  ( -7.474202570535965151, 30.60042966911705165, 3.000000000000023537 ) ) ;
#1257 = DIRECTION ( 'NONE',  ( 0.000000000000000000, 0.000000000000000000, -1.000000000000000000 ) ) ;
#1258 = EDGE_CURVE ( 'NONE', #19899, #11765, #2874, .T. ) ;
#1259 = ORIENTED_EDGE ( 'NONE', *, *, #15717, .F. ) ;
#1260 =( REPRESENTATION_RELATIONSHIP ('NONE','NONE', #8442, #18960 ) REPRESENTATION_RELATIONSHIP_WITH_TRANSFORMATION ( #16961 )SHAPE_REPRESENTATION_RELATIONSHIP( ) );
#1261 = CARTESIAN_POINT ( 'NONE',  ( 2.220446049250313081E-13, -8.326672684688674053E-14, 2.800654218530498785 ) ) ;
#1262 = DIRECTION ( 'NONE',  ( -1.000000000000000000, 0.000000000000000000, 0.000000000000000000 ) ) ;
#1263 = VECTOR ( 'NONE', #7771, 1000.000000000000000 ) ;
#1264 = EDGE_CURVE ( 'NONE', #4080, #2931, #22007, .T. ) ;
#1265 = ORIENTED_EDGE ( 'NONE', *, *, #20237, .T. ) ;
#1266 = B_SPLINE_CURVE_WITH_KNOTS ( 'NONE', 3,
 ( #10601, #3981, #8893, #7520 ),
 .UNSPECIFIED., .F., .F.,
 ( 4, 4 ),
 ( 0.001893031756885373267, 0.003808480026563830501 ),
 .UNSPECIFIED. ) ;
#1267 = ORIENTED_EDGE ( 'NONE', *, *, #13329, .F. ) ;
#1268 = SHAPE_DEFINITION_REPRESENTATION ( #11514, #21292 ) ;
#1269 = B_SPLINE_CURVE_WITH_KNOTS ( 'NONE', 3,
 ( #20292, #4596, #1147, #15100, #20405, #4714 ),
 .UNSPECIFIED., .F., .F.,
 ( 4, 2, 4 ),
 ( 1.116583492552567205E-17, 0.005389490931280165216, 0.01077898186256031829 ),
 .UNSPECIFIED. ) ;
#1270 = EDGE_LOOP ( 'NONE', ( #4084, #14632, #16343, #5836 ) ) ;
#1271 = CYLINDRICAL_SURFACE ( 'NONE', #19822, 1.000000000000000888 ) ;
#1272 = LINE ( 'NONE', #4387, #9795 ) ;
#1273 = CARTESIAN_POINT ( 'NONE',  ( -34.99999999999999289, -1.000000000000028644, -3.012171160963566127E-14 ) ) ;
#1274 = CARTESIAN_POINT ( 'NONE',  ( 34.99999999999980815, 40.00000000000000711, 54.99999999999922551 ) ) ;
#1275 = CIRCLE ( 'NONE', #14789, 36.76383501243555685 ) ;
#1276 = CARTESIAN_POINT ( 'NONE',  ( -19.99999999999998934, 4.500000000000009770, 0.000000000000000000 ) ) ;
#1277 = VERTEX_POINT ( 'NONE', #9857 ) ;
#1278 = CARTESIAN_POINT ( 'NONE',  ( -35.00000000000000000, 17.00000000000000000, 41.00000000000002132 ) ) ;
#1279 = LINE ( 'NONE', #2904, #17100 ) ;
#1280 = ORIENTED_EDGE ( 'NONE', *, *, #921, .F. ) ;
#1281 = DIRECTION ( 'NONE',  ( -1.000000000000000000, 0.000000000000000000, 0.000000000000000000 ) ) ;
#1282 = FACE_BOUND ( 'NONE', #19366, .T. ) ;
#1283 = VECTOR ( 'NONE', #11816, 1000.000000000000000 ) ;
#1284 = CARTESIAN_POINT ( 'NONE',  ( -28.45046755804880689, 15.62726112422596714, -2.999999999999999112 ) ) ;
#1285 = CARTESIAN_POINT ( 'NONE',  ( 8.847970474273168406, 40.00000000000000711, 53.28481329029794011 ) ) ;
#1286 = VERTEX_POINT ( 'NONE', #20172 ) ;
#1287 = CARTESIAN_POINT ( 'NONE',  ( -8.197131438766653844, 40.00000000000000711, -53.04141935927233931 ) ) ;
#1288 = ORIENTED_EDGE ( 'NONE', *, *, #21257, .T. ) ;
#1289 = DIRECTION ( 'NONE',  ( -0.000000000000000000, -0.000000000000000000, 1.000000000000000000 ) ) ;
#1290 = CARTESIAN_POINT ( 'NONE',  ( -6.626710883749606351E-15, -0.4099546584827634121, -48.99240008041271466 ) ) ;
#1291 = ORIENTED_EDGE ( 'NONE', *, *, #4150, .T. ) ;
#1292 = CARTESIAN_POINT ( 'NONE',  ( 4.898587196589407898E-16, 15.00000000000000355, -3.999999999999994671 ) ) ;
#1293 = DIRECTION ( 'NONE',  ( -1.000000000000000000, -1.788446540656407938E-15, 0.000000000000000000 ) ) ;
#1294 = DIRECTION ( 'NONE',  ( -1.000000000000000000, 0.000000000000000000, 0.000000000000000000 ) ) ;
#1295 = EDGE_CURVE ( 'NONE', #11321, #18787, #22415, .T. ) ;
#1296 = CARTESIAN_POINT ( 'NONE',  ( 21.83670385715308271, 14.52494903933254911, -58.53909266577284143 ) ) ;
#1297 = VERTEX_POINT ( 'NONE', #14988 ) ;
#1298 = CIRCLE ( 'NONE', #18126, 2.099999999999997868 ) ;
#1299 = ORIENTED_EDGE ( 'NONE', *, *, #14707, .F. ) ;
#1300 = ORIENTED_EDGE ( 'NONE', *, *, #1610, .F. ) ;
#1301 = PLANE ( 'NONE',  #6546 ) ;
#1302 = ORIENTED_EDGE ( 'NONE', *, *, #10885, .T. ) ;
#1303 = DIRECTION ( 'NONE',  ( 1.000000000000000000, 0.000000000000000000, 0.000000000000000000 ) ) ;
#1304 = DIRECTION ( 'NONE',  ( 6.505213034913038160E-19, 3.903127820947822896E-18, 1.000000000000000000 ) ) ;
#1305 = EDGE_CURVE ( 'NONE', #5648, #21174, #12867, .T. ) ;
#1306 = ORIENTED_EDGE ( 'NONE', *, *, #1183, .F. ) ;
#1307 = CARTESIAN_POINT ( 'NONE',  ( -29.75120097320039392, -20.55056392469606408, -2.932164912090505116 ) ) ;
#1308 = CARTESIAN_POINT ( 'NONE',  ( -6.661198439252719261, -4.819795714544886422, -49.67388352366067750 ) ) ;
#1309 = ORIENTED_EDGE ( 'NONE', *, *, #20125, .F. ) ;
#1310 = VECTOR ( 'NONE', #7238, 1000.000000000000000 ) ;
#1311 = LINE ( 'NONE', #8305, #19049 ) ;
#1312 = CIRCLE ( 'NONE', #2406, 2.500000000000002220 ) ;
#1313 = VECTOR ( 'NONE', #19787, 1000.000000000000000 ) ;
#1314 = VERTEX_POINT ( 'NONE', #11574 ) ;
#1315 = CARTESIAN_POINT ( 'NONE',  ( 5.204790488456048969, 39.83796511861606859, -52.32473449166996460 ) ) ;
#1316 = AXIS2_PLACEMENT_3D ( 'NONE', #12247, #4233, #13025 ) ;
#1317 = DIRECTION ( 'NONE',  ( -1.000000000000000000, 0.000000000000000000, 0.000000000000000000 ) ) ;
#1318 = EDGE_CURVE ( 'NONE', #4146, #3268, #16945, .T. ) ;
#1319 = LINE ( 'NONE', #19080, #8620 ) ;
#1320 = EDGE_CURVE ( 'NONE', #19781, #3437, #5567, .T. ) ;
#1321 = LINE ( 'NONE', #11407, #12067 ) ;
#1322 = AXIS2_PLACEMENT_3D ( 'NONE', #7206, #7552, #15901 ) ;
#1323 = CARTESIAN_POINT ( 'NONE',  ( -9.855264211176372413, 8.670295722316108566, 43.22210574525161064 ) ) ;
#1324 = AXIS2_PLACEMENT_3D ( 'NONE', #6164, #9590, #20145 ) ;
#1325 = ORIENTED_EDGE ( 'NONE', *, *, #20988, .T. ) ;
#1326 = AXIS2_PLACEMENT_3D ( 'NONE', #12628, #3503, #21247 ) ;
#1327 = ORIENTED_EDGE ( 'NONE', *, *, #3809, .T. ) ;
#1328 = ORIENTED_EDGE ( 'NONE', *, *, #519, .T. ) ;
#1329 = ORIENTED_EDGE ( 'NONE', *, *, #637, .T. ) ;
#1330 = CARTESIAN_POINT ( 'NONE',  ( -22.43750227530606978, 20.33721733311116253, 58.67013217117688839 ) ) ;
#1331 = AXIS2_PLACEMENT_3D ( 'NONE', #5809, #12782, #5471 ) ;
#1332 = CYLINDRICAL_SURFACE ( 'NONE', #21333, 22.00000000000000000 ) ;
#1333 = EDGE_CURVE ( 'NONE', #7707, #18834, #16846, .T. ) ;
#1334 = CARTESIAN_POINT ( 'NONE',  ( 7.310544252644470693E-15, 28.19616000222403684, 0.000000000000000000 ) ) ;
#1335 = CARTESIAN_POINT ( 'NONE',  ( -11.16030968682941804, 40.00000000000000000, 54.02479386262969996 ) ) ;
#1336 = CARTESIAN_POINT ( 'NONE',  ( 2.220446049250313081E-13, -2.498001805406602216E-13, -6.859353255829918616 ) ) ;
#1337 = EDGE_LOOP ( 'NONE', ( #4788, #4078 ) ) ;
#1338 = DIRECTION ( 'NONE',  ( 6.505213034913038160E-19, 3.903127820947822896E-18, 1.000000000000000000 ) ) ;
#1339 = CARTESIAN_POINT ( 'NONE',  ( -6.019227127673981492, 39.99999999999999289, -52.10376796897383400 ) ) ;
#1340 = EDGE_CURVE ( 'NONE', #7376, #22334, #6534, .T. ) ;
#1341 = CARTESIAN_POINT ( 'NONE',  ( -10.00000000000000000, 1.499999999999997780, 3.000000000000000000 ) ) ;
#1342 = EDGE_CURVE ( 'NONE', #6332, #11390, #20202, .T. ) ;
#1343 = LINE ( 'NONE', #15307, #2031 ) ;
#1344 = CIRCLE ( 'NONE', #21481, 0.9999999999999974465 ) ;
#1345 = ORIENTED_EDGE ( 'NONE', *, *, #1728, .F. ) ;
#1346 = DIRECTION ( 'NONE',  ( -0.000000000000000000, -1.000000000000000000, -0.000000000000000000 ) ) ;
#1347 = AXIS2_PLACEMENT_3D ( 'NONE', #14150, #308, #21281 ) ;
#1348 = ORIENTED_EDGE ( 'NONE', *, *, #7352, .T. ) ;
#1349 = CARTESIAN_POINT ( 'NONE',  ( -1.423424233832348840, -32.35999952201584762, 3.000000000000002665 ) ) ;
#1350 = DIRECTION ( 'NONE',  ( 0.000000000000000000, 0.000000000000000000, -1.000000000000000000 ) ) ;
#1351 = CARTESIAN_POINT ( 'NONE',  ( -34.99999999999999289, 0.000000000000000000, -54.99999999999705125 ) ) ;
#1352 = DIRECTION ( 'NONE',  ( 0.000000000000000000, 0.000000000000000000, -1.000000000000000000 ) ) ;
#1353 = ADVANCED_FACE ( 'NONE', ( #1144 ), #2535, .T. ) ;
#1354 = ORIENTED_EDGE ( 'NONE', *, *, #11440, .T. ) ;
#1355 = VECTOR ( 'NONE', #1852, 1000.000000000000000 ) ;
#1356 = VECTOR ( 'NONE', #9848, 1000.000000000000000 ) ;
#1357 = ORIENTED_EDGE ( 'NONE', *, *, #7511, .T. ) ;
#1358 = DIRECTION ( 'NONE',  ( -0.000000000000000000, 1.000000000000000000, -0.000000000000000000 ) ) ;
#1359 = FACE_OUTER_BOUND ( 'NONE', #5225, .T. ) ;
#1360 = ORIENTED_EDGE ( 'NONE', *, *, #8232, .F. ) ;
#1361 = DIRECTION ( 'NONE',  ( 0.000000000000000000, 0.000000000000000000, 1.000000000000000000 ) ) ;
#1362 = CARTESIAN_POINT ( 'NONE',  ( -5.833333333333341919, 33.81926995981417150, -40.61164310337066041 ) ) ;
#1363 = LINE ( 'NONE', #3328, #8712 ) ;
#1364 = CARTESIAN_POINT ( 'NONE',  ( -20.31722544680652476, 29.72987180553229791, -58.17992760854140499 ) ) ;
#1365 = DIRECTION ( 'NONE',  ( 6.505213034913038160E-19, 3.903127820947822896E-18, 1.000000000000000000 ) ) ;
#1366 = AXIS2_PLACEMENT_3D ( 'NONE', #3464, #14075, #10640 ) ;
#1367 = CARTESIAN_POINT ( 'NONE',  ( -16.64903669413044085, 31.11586081922098757, 59.71532480898648743 ) ) ;
#1368 = VERTEX_POINT ( 'NONE', #9520 ) ;
#1369 = DIRECTION ( 'NONE',  ( -0.000000000000000000, -1.000000000000000000, -0.000000000000000000 ) ) ;
#1370 = AXIS2_PLACEMENT_3D ( 'NONE', #22005, #13158, #11571 ) ;
#1371 = CARTESIAN_POINT ( 'NONE',  ( 12.84005703541281207, 1.693876179768766699, -55.76322220626109072 ) ) ;
#1372 = CARTESIAN_POINT ( 'NONE',  ( 6.696867368503558448E-15, 40.00000000000000000, 39.73397172404484223 ) ) ;
#1373 = VECTOR ( 'NONE', #12449, 1000.000000000000000 ) ;
#1374 = EDGE_CURVE ( 'NONE', #21043, #20280, #14319, .T. ) ;
#1375 = ORIENTED_EDGE ( 'NONE', *, *, #8971, .T. ) ;
#1376 = DIRECTION ( 'NONE',  ( 0.4124789556921644729, -0.7071067811865296981, -0.5743353646704393300 ) ) ;
#1377 = EDGE_CURVE ( 'NONE', #9166, #8764, #11774, .T. ) ;
#1378 = DIRECTION ( 'NONE',  ( 6.505213034913038160E-19, 3.903127820947822896E-18, 1.000000000000000000 ) ) ;
#1379 = CARTESIAN_POINT ( 'NONE',  ( 24.03323817228492132, -20.36304159388363644, 2.999999999999995559 ) ) ;
#1380 = DIRECTION ( 'NONE',  ( -1.000000000000000000, -1.208970125616060717E-17, 0.000000000000000000 ) ) ;
#1381 = AXIS2_PLACEMENT_3D ( 'NONE', #8599, #1617, #10533 ) ;
#1382 = EDGE_CURVE ( 'NONE', #2473, #2421, #19105, .T. ) ;
#1383 = VERTEX_POINT ( 'NONE', #18561 ) ;
#1384 = CIRCLE ( 'NONE', #21527, 3.999999999999996447 ) ;
#1385 = ORIENTED_EDGE ( 'NONE', *, *, #21758, .T. ) ;
#1386 = CIRCLE ( 'NONE', #14175, 17.00000000000000000 ) ;
#1387 = ORIENTED_EDGE ( 'NONE', *, *, #1673, .T. ) ;
#1388 = CARTESIAN_POINT ( 'NONE',  ( 14.67611967928938910, -31.67162468656004037, 2.999999999999999112 ) ) ;
#1389 = CARTESIAN_POINT ( 'NONE',  ( 3.174475770757817727, -4.645331003331005348, 47.72510079651066661 ) ) ;
#1390 = CARTESIAN_POINT ( 'NONE',  ( -34.99999999999980815, 39.97500000000000142, 54.99999999999922551 ) ) ;
#1391 = CARTESIAN_POINT ( 'NONE',  ( -28.88846368933341324, -19.59430950039328678, 2.999999999999995559 ) ) ;
#1392 = CARTESIAN_POINT ( 'NONE',  ( -26.00000000000001421, 19.99999999999982947, -105.0010000000000048 ) ) ;
#1393 = ORIENTED_EDGE ( 'NONE', *, *, #3282, .F. ) ;
#1394 = DIRECTION ( 'NONE',  ( 6.505213034913038160E-19, 3.903127820947822896E-18, 1.000000000000000000 ) ) ;
#1395 = CARTESIAN_POINT ( 'NONE',  ( -11.51194040402259233, 39.05862814753313472, 55.21283662269736681 ) ) ;
#1396 = ORIENTED_EDGE ( 'NONE', *, *, #848, .F. ) ;
#1397 = FACE_OUTER_BOUND ( 'NONE', #4955, .T. ) ;
#1398 = DIRECTION ( 'NONE',  ( 0.000000000000000000, 0.000000000000000000, 1.000000000000000000 ) ) ;
#1399 = APPLICATION_CONTEXT ( 'automotive_design' ) ;
#1400 = EDGE_CURVE ( 'NONE', #5811, #2517, #8137, .T. ) ;
#1401 = CARTESIAN_POINT ( 'NONE',  ( -5.999999999999998224, 20.00000000000000000, 5.999999999999999112 ) ) ;
#1402 = LINE ( 'NONE', #8610, #11556 ) ;
#1403 = EDGE_LOOP ( 'NONE', ( #1123, #13567, #12653, #15852 ) ) ;
#1404 = CARTESIAN_POINT ( 'NONE',  ( 11.84374239103369142, 29.21200678190360378, -44.31542800769554447 ) ) ;
#1405 = AXIS2_PLACEMENT_3D ( 'NONE', #1465, #5570, #5468 ) ;
#1406 = ORIENTED_EDGE ( 'NONE', *, *, #8971, .F. ) ;
#1407 = CARTESIAN_POINT ( 'NONE',  ( 21.05198877411829272, -30.13956425491240410, -2.800654218530457484 ) ) ;
#1408 = DIRECTION ( 'NONE',  ( 1.000000000000000000, 0.000000000000000000, 0.000000000000000000 ) ) ;
#1409 = AXIS2_PLACEMENT_3D ( 'NONE', #1876, #7030, #17340 ) ;
#1410 = ORIENTED_EDGE ( 'NONE', *, *, #4917, .F. ) ;
#1411 = FACE_OUTER_BOUND ( 'NONE', #8286, .T. ) ;
#1412 = AXIS2_PLACEMENT_3D ( 'NONE', #14691, #11146, #21698 ) ;
#1413 = AXIS2_PLACEMENT_3D ( 'NONE', #7347, #12483, #462 ) ;
#1414 = DIRECTION ( 'NONE',  ( 6.505213034913038160E-19, 3.903127820947822896E-18, 1.000000000000000000 ) ) ;
#1415 = CARTESIAN_POINT ( 'NONE',  ( 0.8626474017861728294, 36.14481870267503894, 2.932969818539059137 ) ) ;
#1416 = CIRCLE ( 'NONE', #9481, 30.00000000000000000 ) ;
#1417 = CARTESIAN_POINT ( 'NONE',  ( 18.43720426448665961, 27.80056269872056163, -57.71457384194849993 ) ) ;
#1418 = VERTEX_POINT ( 'NONE', #6415 ) ;
#1419 = ORIENTED_EDGE ( 'NONE', *, *, #5332, .F. ) ;
#1420 = AXIS2_PLACEMENT_3D ( 'NONE', #20372, #8111, #1118 ) ;
#1421 = ORIENTED_EDGE ( 'NONE', *, *, #8605, .F. ) ;
#1422 = EDGE_CURVE ( 'NONE', #6590, #6061, #10662, .T. ) ;
#1423 = ORIENTED_EDGE ( 'NONE', *, *, #18959, .T. ) ;
#1424 = DIRECTION ( 'NONE',  ( 0.000000000000000000, 0.000000000000000000, -1.000000000000000000 ) ) ;
#1425 = DIRECTION ( 'NONE',  ( -0.000000000000000000, -1.000000000000000000, -0.000000000000000000 ) ) ;
#1426 = DIRECTION ( 'NONE',  ( 0.000000000000000000, 1.000000000000000000, 0.000000000000000000 ) ) ;
#1427 = ORIENTED_EDGE ( 'NONE', *, *, #4182, .T. ) ;
#1428 = CARTESIAN_POINT ( 'NONE',  ( 42.50000000000000711, -12.00000000000000000, 49.60000000000000853 ) ) ;
#1429 = CARTESIAN_POINT ( 'NONE',  ( 2.999964809120486908, 15.80129619923657103, 6.485293816093339103 ) ) ;
#1430 = ORIENTED_EDGE ( 'NONE', *, *, #18003, .T. ) ;
#1431 = AXIS2_PLACEMENT_3D ( 'NONE', #12836, #4609, #9639 ) ;
#1432 = CARTESIAN_POINT ( 'NONE',  ( 35.00000000000000000, 14.00000000000000000, -38.99999999999997868 ) ) ;
#1433 = ADVANCED_FACE ( 'NONE', ( #20613 ), #4310, .F. ) ;
#1434 = VERTEX_POINT ( 'NONE', #8542 ) ;
#1435 = LINE ( 'NONE', #12088, #8258 ) ;
#1436 = CARTESIAN_POINT ( 'NONE',  ( 20.00000000000000000, 28.19616000222403329, 2.449293598294705724E-15 ) ) ;
#1437 = CARTESIAN_POINT ( 'NONE',  ( 29.75120097320059642, 20.55056392469582249, -2.932164912090509556 ) ) ;
#1438 = CARTESIAN_POINT ( 'NONE',  ( -1.044209099552145581, 39.99351895515111011, 49.52925835065091320 ) ) ;
#1439 = TOROIDAL_SURFACE ( 'NONE', #14213, 34.90673715956759082, 8.750000000000000000 ) ;
#1440 = LINE ( 'NONE', #14853, #8918 ) ;
#1441 = CIRCLE ( 'NONE', #7651, 19.11328065563151668 ) ;
#1442 = CARTESIAN_POINT ( 'NONE',  ( 18.83615802559807051, -32.14641817400198676, -2.999999999999950706 ) ) ;
#1443 = ADVANCED_FACE ( 'NONE', ( #5341 ), #12144, .F. ) ;
#1444 =( GEOMETRIC_REPRESENTATION_CONTEXT ( 3 ) GLOBAL_UNCERTAINTY_ASSIGNED_CONTEXT ( ( #13302 ) ) GLOBAL_UNIT_ASSIGNED_CONTEXT ( ( #598, #9306, #250 ) ) REPRESENTATION_CONTEXT ( 'NONE', 'WORKASPACE' ) );
#1445 = ORIENTED_EDGE ( 'NONE', *, *, #22074, .T. ) ;
#1446 = ORIENTED_EDGE ( 'NONE', *, *, #8571, .T. ) ;
#1447 = ORIENTED_EDGE ( 'NONE', *, *, #21089, .F. ) ;
#1448 = EDGE_CURVE ( 'NONE', #16878, #5871, #5205, .T. ) ;
#1449 = ORIENTED_EDGE ( 'NONE', *, *, #14657, .F. ) ;
#1450 = CARTESIAN_POINT ( 'NONE',  ( -16.35275686153619645, 4.590993025983391540, 57.03319805596881054 ) ) ;
#1451 = LINE ( 'NONE', #20249, #16625 ) ;
#1452 = B_SPLINE_CURVE_WITH_KNOTS ( 'NONE', 3,
 ( #13805, #20822, #11366, #2671 ),
 .UNSPECIFIED., .F., .F.,
 ( 4, 4 ),
 ( 0.000000000000000000, 0.001590342073036659634 ),
 .UNSPECIFIED. ) ;
#1453 = TOROIDAL_SURFACE ( 'NONE', #18647, 34.90673715956759082, 8.750000000000000000 ) ;
#1454 = CARTESIAN_POINT ( 'NONE',  ( 1.080492130498492465, 39.99305441129651228, -49.55624281123191821 ) ) ;
#1455 = CARTESIAN_POINT ( 'NONE',  ( -18.11182660255255428, 11.48022137427004097, -60.14030069439205306 ) ) ;
#1456 = DIRECTION ( 'NONE',  ( -1.000000000000000000, 0.000000000000000000, 0.000000000000000000 ) ) ;
#1457 = ORIENTED_EDGE ( 'NONE', *, *, #7090, .T. ) ;
#1458 = CARTESIAN_POINT ( 'NONE',  ( -35.00000000000058265, 40.00000000000000711, -55.00000000000076028 ) ) ;
#1459 = CARTESIAN_POINT ( 'NONE',  ( -2.321955456489504854, 40.00000000000000000, -50.16149369290168636 ) ) ;
#1460 = CARTESIAN_POINT ( 'NONE',  ( -28.52469787935786982, 10.00000000000000000, -4.095854054471906203 ) ) ;
#1461 = DIRECTION ( 'NONE',  ( 6.505213034913038160E-19, 3.903127820947822896E-18, 1.000000000000000000 ) ) ;
#1462 = ORIENTED_EDGE ( 'NONE', *, *, #22203, .T. ) ;
#1463 = CARTESIAN_POINT ( 'NONE',  ( 29.14949368109903816, -11.93972437435561496, -6.999999999999999112 ) ) ;
#1464 = ORIENTED_EDGE ( 'NONE', *, *, #5972, .F. ) ;
#1465 = CARTESIAN_POINT ( 'NONE',  ( 2.775557561562891351E-14, 2.775557561562891351E-14, 5.750000000000001776 ) ) ;
#1466 = LINE ( 'NONE', #1231, #11872 ) ;
#1467 = EDGE_CURVE ( 'NONE', #8376, #13932, #14012, .T. ) ;
#1468 = AXIS2_PLACEMENT_3D ( 'NONE', #529, #7523, #7638 ) ;
#1469 = DIRECTION ( 'NONE',  ( 1.296372316667914327E-16, 1.000000000000000000, -0.000000000000000000 ) ) ;
#1470 = LINE ( 'NONE', #13928, #19264 ) ;
#1471 = VERTEX_POINT ( 'NONE', #15518 ) ;
#1472 = EDGE_CURVE ( 'NONE', #1729, #5874, #13588, .T. ) ;
#1473 = ORIENTED_EDGE ( 'NONE', *, *, #8027, .T. ) ;
#1474 = CARTESIAN_POINT ( 'NONE',  ( -8.309432361859336424, 0.006312382049299974755, 53.49092837495744845 ) ) ;
#1475 = TOROIDAL_SURFACE ( 'NONE', #2955, 34.90673715956759082, 8.750000000000000000 ) ;
#1476 = CARTESIAN_POINT ( 'NONE',  ( 2.602085213965210642E-15, 0.6398376396478597794, 0.000000000000000000 ) ) ;
#1477 = ORIENTED_EDGE ( 'NONE', *, *, #17589, .F. ) ;
#1478 = CARTESIAN_POINT ( 'NONE',  ( 14.40375226887234206, 15.79546342576956164, 45.56106839101555295 ) ) ;
#1479 = ADVANCED_FACE ( 'NONE', ( #4888 ), #22667, .F. ) ;
#1480 = DIRECTION ( 'NONE',  ( -0.000000000000000000, -0.000000000000000000, -1.000000000000000000 ) ) ;
#1481 = DIRECTION ( 'NONE',  ( -0.000000000000000000, 1.000000000000000000, -0.000000000000000000 ) ) ;
#1482 = CARTESIAN_POINT ( 'NONE',  ( -22.42250004520216677, 20.31170080112651277, -58.66691407552180237 ) ) ;
#1483 = CARTESIAN_POINT ( 'NONE',  ( -31.09841355225970005, 5.093313992686310243, 2.999999999999995559 ) ) ;
#1484 = EDGE_CURVE ( 'NONE', #1150, #5679, #16906, .T. ) ;
#1485 = CARTESIAN_POINT ( 'NONE',  ( -8.331955809010626268, 38.18181818181818699, 56.36098470834075158 ) ) ;
#1486 = ORIENTED_EDGE ( 'NONE', *, *, #22195, .T. ) ;
#1487 = CARTESIAN_POINT ( 'NONE',  ( -28.95348479018568355, 14.76298474240497782, -2.999999999999999112 ) ) ;
#1488 =( NAMED_UNIT ( * ) PLANE_ANGLE_UNIT ( ) SI_UNIT ( $, .RADIAN. ) );
#1489 = LINE ( 'NONE', #13265, #7925 ) ;
#1490 = FACE_OUTER_BOUND ( 'NONE', #12539, .T. ) ;
#1491 = EDGE_LOOP ( 'NONE', ( #5886, #13429, #17032, #22013, #13605, #1325 ) ) ;
#1492 = VECTOR ( 'NONE', #14249, 1000.000000000000000 ) ;
#1493 = EDGE_CURVE ( 'NONE', #19154, #7411, #3753, .T. ) ;
#1494 = DIRECTION ( 'NONE',  ( 0.000000000000000000, -0.7071067811865302533, -0.7071067811865647812 ) ) ;
#1495 = DIRECTION ( 'NONE',  ( 0.000000000000000000, 0.000000000000000000, -1.000000000000000000 ) ) ;
#1496 = CARTESIAN_POINT ( 'NONE',  ( -36.54278193890292670, -4.025500340002762911, -1.999999999999977573 ) ) ;
#1497 = ORIENTED_EDGE ( 'NONE', *, *, #12359, .T. ) ;
#1498 = SHAPE_DEFINITION_REPRESENTATION ( #16442, #18960 ) ;
#1499 = EDGE_CURVE ( 'NONE', #11018, #12118, #6669, .T. ) ;
#1500 = VERTEX_POINT ( 'NONE', #10137 ) ;
#1501 = CARTESIAN_POINT ( 'NONE',  ( -40.40000000000001279, -9.600000000000001421, -47.50000000000000000 ) ) ;
#1502 = CARTESIAN_POINT ( 'NONE',  ( -1.564319729173390128, -1.162775034690427534, 47.08282483555631615 ) ) ;
#1503 = AXIS2_PLACEMENT_3D ( 'NONE', #16634, #6320, #941 ) ;
#1504 = DIRECTION ( 'NONE',  ( 0.000000000000000000, 1.000000000000000000, 0.000000000000000000 ) ) ;
#1505 = EDGE_CURVE ( 'NONE', #15515, #14562, #11061, .T. ) ;
#1506 = FACE_BOUND ( 'NONE', #395, .T. ) ;
#1507 = DIRECTION ( 'NONE',  ( -1.000000000000000000, -1.208970125616081209E-17, 0.000000000000000000 ) ) ;
#1508 = VERTEX_POINT ( 'NONE', #1900 ) ;
#1509 = DIRECTION ( 'NONE',  ( 0.000000000000000000, 0.000000000000000000, -1.000000000000000000 ) ) ;
#1510 = CARTESIAN_POINT ( 'NONE',  ( -31.41173278719225337, -17.66631876130930578, -2.999999999999981792 ) ) ;
#1511 = ORIENTED_EDGE ( 'NONE', *, *, #14720, .F. ) ;
#1512 = CARTESIAN_POINT ( 'NONE',  ( 4.104166344909097042, -35.92356703407504881, 2.932460736555814407 ) ) ;
#1513 = DIRECTION ( 'NONE',  ( -1.000000000000000000, -1.208970125616083212E-17, 0.000000000000000000 ) ) ;
#1514 = DIRECTION ( 'NONE',  ( -0.000000000000000000, -1.000000000000000000, -0.000000000000000000 ) ) ;
#1515 = CARTESIAN_POINT ( 'NONE',  ( 4.996179657326272228, 39.84467275760181337, 52.21079474515372709 ) ) ;
#1516 = ORIENTED_EDGE ( 'NONE', *, *, #3101, .T. ) ;
#1517 = CARTESIAN_POINT ( 'NONE',  ( 11.37797799463863591, 29.78145794493465459, -44.06891764425670033 ) ) ;
#1518 = EDGE_CURVE ( 'NONE', #8421, #11018, #19211, .T. ) ;
#1519 = ORIENTED_EDGE ( 'NONE', *, *, #4640, .F. ) ;
#1520 = CARTESIAN_POINT ( 'NONE',  ( -7.882609639814679786E-15, -9.552912840896525389E-26, -50.50395615645409464 ) ) ;
#1521 = DIRECTION ( 'NONE',  ( 1.000000000000000000, 0.000000000000000000, 0.000000000000000000 ) ) ;
#1522 = EDGE_LOOP ( 'NONE', ( #3610, #7248, #14036, #10775 ) ) ;
#1523 = DIRECTION ( 'NONE',  ( 0.000000000000000000, 0.000000000000000000, -1.000000000000000000 ) ) ;
#1524 = AXIS2_PLACEMENT_3D ( 'NONE', #5066, #8595, #12043 ) ;
#1525 = AXIS2_PLACEMENT_3D ( 'NONE', #8048, #13175, #16519 ) ;
#1526 = DIRECTION ( 'NONE',  ( -1.000000000000000000, 1.927470528863119049E-16, 0.000000000000000000 ) ) ;
#1527 = DIRECTION ( 'NONE',  ( 1.049727191138618326E-16, -0.5150380749100547106, 0.8571673007021120005 ) ) ;
#1528 = DIRECTION ( 'NONE',  ( -1.445602896647339163E-16, -0.000000000000000000, -1.000000000000000000 ) ) ;
#1529 = ORIENTED_EDGE ( 'NONE', *, *, #2995, .T. ) ;
#1530 = ORIENTED_EDGE ( 'NONE', *, *, #20547, .F. ) ;
#1531 = ORIENTED_EDGE ( 'NONE', *, *, #14736, .T. ) ;
#1532 = ADVANCED_FACE ( 'NONE', ( #10360 ), #2668, .F. ) ;
#1533 = ORIENTED_EDGE ( 'NONE', *, *, #11163, .F. ) ;
#1534 = DIRECTION ( 'NONE',  ( -6.505213034913038160E-19, -3.903127820947822896E-18, -1.000000000000000000 ) ) ;
#1535 = CARTESIAN_POINT ( 'NONE',  ( 19.75454541434352862, 30.69619330606318997, 58.03277863335249975 ) ) ;
#1536 = VECTOR ( 'NONE', #1251, 1000.000000000000000 ) ;
#1537 = CARTESIAN_POINT ( 'NONE',  ( 7.763914066288519322, 40.00000000000000711, -52.86923209262808854 ) ) ;
#1538 = VERTEX_POINT ( 'NONE', #18865 ) ;
#1539 = CARTESIAN_POINT ( 'NONE',  ( -90.00000000000000000, 40.00000000000000000, -2.099999999999991651 ) ) ;
#1540 = FACE_OUTER_BOUND ( 'NONE', #15792, .T. ) ;
#1541 = ORIENTED_EDGE ( 'NONE', *, *, #20668, .T. ) ;
#1542 = CARTESIAN_POINT ( 'NONE',  ( -6.976160265002656402, 1.175630724176373931, 53.22984522349711511 ) ) ;
#1543 = CARTESIAN_POINT ( 'NONE',  ( 35.00000000000002132, -5.000000000000000000, -59.99999999999703704 ) ) ;
#1544 = ORIENTED_EDGE ( 'NONE', *, *, #3658, .T. ) ;
#1545 = CARTESIAN_POINT ( 'NONE',  ( 8.620000862318205392, 38.06588505537628464, -54.65497975194055869 ) ) ;
#1546 = DIRECTION ( 'NONE',  ( 0.000000000000000000, 1.000000000000000000, 0.000000000000000000 ) ) ;
#1547 = FACE_OUTER_BOUND ( 'NONE', #14907, .T. ) ;
#1548 = CARTESIAN_POINT ( 'NONE',  ( -7.213741798857487453, 39.66007640230202469, 53.46061959581572154 ) ) ;
#1549 = FACE_OUTER_BOUND ( 'NONE', #14128, .T. ) ;
#1550 = EDGE_CURVE ( 'NONE', #10325, #15602, #6308, .T. ) ;
#1551 = CARTESIAN_POINT ( 'NONE',  ( 10.01331137436180008, -34.09180625983483992, -2.999999999999996891 ) ) ;
#1552 = ORIENTED_EDGE ( 'NONE', *, *, #2402, .F. ) ;
#1553 = EDGE_CURVE ( 'NONE', #2190, #14890, #85, .T. ) ;
#1554 = ORIENTED_EDGE ( 'NONE', *, *, #11138, .F. ) ;
#1555 = VERTEX_POINT ( 'NONE', #3516 ) ;
#1556 = EDGE_LOOP ( 'NONE', ( #12338, #1541, #14784, #10779 ) ) ;
#1557 = CARTESIAN_POINT ( 'NONE',  ( 2.220446049250313081E-13, -8.326672684688674053E-14, 2.800654218530498785 ) ) ;
#1558 = DIRECTION ( 'NONE',  ( 0.9898477157360406897, 0.000000000000000000, -0.1421319796954317316 ) ) ;
#1559 = CARTESIAN_POINT ( 'NONE',  ( -34.99999999999999289, -5.000000000000000000, -52.49999999999705125 ) ) ;
#1560 = CARTESIAN_POINT ( 'NONE',  ( -18.43548664438527851, 12.20444905678966308, -60.22785496272550176 ) ) ;
#1561 = CARTESIAN_POINT ( 'NONE',  ( 0.5103185168914748937, 39.99845979616902270, 49.12706063236587539 ) ) ;
#1562 = AXIS2_PLACEMENT_3D ( 'NONE', #2038, #14391, #17621 ) ;
#1563 = VECTOR ( 'NONE', #2236, 1000.000000000000000 ) ;
#1564 = ORIENTED_EDGE ( 'NONE', *, *, #14623, .T. ) ;
#1565 = DIRECTION ( 'NONE',  ( 0.000000000000000000, -1.000000000000000000, 0.000000000000000000 ) ) ;
#1566 = B_SPLINE_CURVE_WITH_KNOTS ( 'NONE', 3,
 ( #21891, #18094, #6068, #20054, #2642, #9614 ),
 .UNSPECIFIED., .F., .F.,
 ( 4, 2, 4 ),
 ( 0.5000000000000000000, 0.7500000000000000000, 1.000000000000000000 ),
 .UNSPECIFIED. ) ;
#1567 = DIRECTION ( 'NONE',  ( -0.1421319796954317316, 0.000000000000000000, 0.9898477157360405787 ) ) ;
#1568 = CARTESIAN_POINT ( 'NONE',  ( 12.24744603030438839, 40.00000000000000000, -54.43639671998947449 ) ) ;
#1569 = CIRCLE ( 'NONE', #12525, 19.11328065563151668 ) ;
#1570 = ORIENTED_EDGE ( 'NONE', *, *, #10768, .F. ) ;
#1571 = CARTESIAN_POINT ( 'NONE',  ( -18.52604901273059212, 27.59774142807035346, 60.25307787776294077 ) ) ;
#1572 = ADVANCED_FACE ( 'NONE', ( #20929 ), #20220, .F. ) ;
#1573 = ORIENTED_EDGE ( 'NONE', *, *, #1493, .T. ) ;
#1574 = CARTESIAN_POINT ( 'NONE',  ( -6.000000000000000000, -20.00000000000000000, -5.999999999999999112 ) ) ;
#1575 = CARTESIAN_POINT ( 'NONE',  ( -35.00000000000000000, 17.00000000000000000, 2.365113165210053967E-14 ) ) ;
#1576 = CARTESIAN_POINT ( 'NONE',  ( -42.50000000000000711, -11.97499999999999964, 47.50000000000000711 ) ) ;
#1577 = ORIENTED_EDGE ( 'NONE', *, *, #20768, .F. ) ;
#1578 = ADVANCED_FACE ( 'NONE', ( #21038 ), #21605, .F. ) ;
#1579 = VECTOR ( 'NONE', #452, 1000.000000000000000 ) ;
#1580 = AXIS2_PLACEMENT_3D ( 'NONE', #3741, #21487, #2586 ) ;
#1581 = COLOUR_RGB ( '',0.7921568627450980005, 0.8196078431372548767, 0.9333333333333333481 ) ;
#1582 = ORIENTED_EDGE ( 'NONE', *, *, #6936, .F. ) ;
#1583 = DIRECTION ( 'NONE',  ( -1.000000000000000000, 0.000000000000000000, 0.000000000000000000 ) ) ;
#1584 = CARTESIAN_POINT ( 'NONE',  ( 32.09841355226000559, -5.093313992686670844, 2.999999999999995559 ) ) ;
#1585 = ORIENTED_EDGE ( 'NONE', *, *, #10418, .T. ) ;
#1586 = CARTESIAN_POINT ( 'NONE',  ( 5.833333333333339255, 6.180730040185842711, 40.61164310337068173 ) ) ;
#1587 = ADVANCED_FACE ( 'NONE', ( #15973 ), #12644, .T. ) ;
#1588 = CARTESIAN_POINT ( 'NONE',  ( 22.97438720605751783, -22.98755168577440600, -2.999999999999995559 ) ) ;
#1589 = DIRECTION ( 'NONE',  ( 3.063596499322170048E-16, 0.000000000000000000, 1.000000000000000000 ) ) ;
#1590 = CARTESIAN_POINT ( 'NONE',  ( -22.42386962120398408, 19.82082524447363525, -58.66720683610021325 ) ) ;
#1591 = CARTESIAN_POINT ( 'NONE',  ( 18.22261011550299514, 31.92986134326217140, -2.800654218530460593 ) ) ;
#1592 = B_SPLINE_SURFACE_WITH_KNOTS ( 'NONE', 1, 3, ( 
 ( #13655, #4977, #1873, #10231, #15611, #12077, #6928, #1537, #15496, #5206, #22516, #7027, #19628, #5423, #9192, #12841, #12735, #10784, #12401, #3936 ),
 ( #8855, #19412, #2209, #14218, #21233, #5525, #11130, #19751, #14332, #1980, #18128, #16167, #3713, #10663, #21340, #8963, #12500, #4055, #15943, #21578 ) ),
 .UNSPECIFIED., .F., .F., .F.,
 ( 2, 2 ),
 ( 4, 2, 2, 2, 2, 2, 2, 2, 2, 4 ),
 ( 0.000000000000000000, 1.000000000000000000 ),
 ( -4.253008135335690669E-05, 0.0006545663507244089139, 0.001351662782802174646, 0.002048759214879940487, 0.002745855646957706328, 0.004140048511113238010, 0.005534241375268769692, 0.006928434239424301373, 0.008322627103579833055, 0.01111101283189089642 ),
 .UNSPECIFIED. ) ;
#1593 = CONICAL_SURFACE ( 'NONE', #11103, 3.399999999999995026, 1.029744258676652313 ) ;
#1594 = EDGE_LOOP ( 'NONE', ( #6227, #6035, #12984, #4629 ) ) ;
#1595 = FACE_OUTER_BOUND ( 'NONE', #17651, .T. ) ;
#1596 = AXIS2_PLACEMENT_3D ( 'NONE', #16018, #10738, #7429 ) ;
#1597 = FACE_BOUND ( 'NONE', #3600, .T. ) ;
#1598 = EDGE_CURVE ( 'NONE', #12848, #7247, #8512, .T. ) ;
#1599 = ADVANCED_FACE ( 'NONE', ( #16200 ), #5577, .F. ) ;
#1600 = CARTESIAN_POINT ( 'NONE',  ( 42.50000000000000711, -9.600000000000001421, -50.00000000000000000 ) ) ;
#1601 = AXIS2_PLACEMENT_3D ( 'NONE', #4261, #18232, #2545 ) ;
#1602 = ORIENTED_EDGE ( 'NONE', *, *, #8075, .T. ) ;
#1603 = CARTESIAN_POINT ( 'NONE',  ( 2.220446049250313081E-13, 2.775557561562891351E-14, -2.800654218530485018 ) ) ;
#1604 = DIRECTION ( 'NONE',  ( 0.000000000000000000, 0.000000000000000000, 1.000000000000000000 ) ) ;
#1605 = CYLINDRICAL_SURFACE ( 'NONE', #682, 3.399999999999995026 ) ;
#1606 = AXIS2_PLACEMENT_3D ( 'NONE', #13672, #20241, #16907 ) ;
#1607 = ADVANCED_FACE ( 'NONE', ( #10937 ), #2474, .F. ) ;
#1608 = VERTEX_POINT ( 'NONE', #17818 ) ;
#1609 = VECTOR ( 'NONE', #8019, 1000.000000000000000 ) ;
#1610 = EDGE_CURVE ( 'NONE', #18860, #9318, #823, .T. ) ;
#1611 = DIRECTION ( 'NONE',  ( 1.000000000000000000, 0.000000000000000000, 0.000000000000000000 ) ) ;
#1612 = AXIS2_PLACEMENT_3D ( 'NONE', #18108, #14771, #16730 ) ;
#1613 = ORIENTED_EDGE ( 'NONE', *, *, #6289, .T. ) ;
#1614 = CARTESIAN_POINT ( 'NONE',  ( 4.170748987303491084, -34.65667543218836499, -2.999999999999988898 ) ) ;
#1615 = CYLINDRICAL_SURFACE ( 'NONE', #8464, 8.999999999999998224 ) ;
#1616 = DIRECTION ( 'NONE',  ( 0.000000000000000000, 1.000000000000000000, 0.000000000000000000 ) ) ;
#1617 = DIRECTION ( 'NONE',  ( 0.000000000000000000, -1.000000000000000000, 0.000000000000000000 ) ) ;
#1618 = EDGE_CURVE ( 'NONE', #18735, #18629, #14479, .T. ) ;
#1619 = LINE ( 'NONE', #3234, #6176 ) ;
#1620 = ORIENTED_EDGE ( 'NONE', *, *, #6633, .F. ) ;
#1621 = DIRECTION ( 'NONE',  ( -0.000000000000000000, -1.000000000000000000, -0.000000000000000000 ) ) ;
#1622 = CARTESIAN_POINT ( 'NONE',  ( -10.43027093729826227, 39.22757009021512431, 54.80615623442511009 ) ) ;
#1623 = ORIENTED_EDGE ( 'NONE', *, *, #10554, .F. ) ;
#1624 = CARTESIAN_POINT ( 'NONE',  ( 3.849727973822421485E-15, 1.499999999999997780, 0.000000000000000000 ) ) ;
#1625 = DIRECTION ( 'NONE',  ( 6.505213034913038160E-19, 3.903127820947822896E-18, 1.000000000000000000 ) ) ;
#1626 = DIRECTION ( 'NONE',  ( 0.000000000000000000, 0.000000000000000000, 1.000000000000000000 ) ) ;
#1627 = CARTESIAN_POINT ( 'NONE',  ( 35.00000000000000000, 25.00000000000000000, -9.000000000000000000 ) ) ;
#1628 = CARTESIAN_POINT ( 'NONE',  ( -9.689843208404349539, 39.33333333333335702, -54.54983754392760886 ) ) ;
#1629 = ORIENTED_EDGE ( 'NONE', *, *, #17873, .F. ) ;
#1630 = LINE ( 'NONE', #18937, #3903 ) ;
#1631 = VECTOR ( 'NONE', #2464, 1000.000000000000000 ) ;
#1632 = ADVANCED_FACE ( 'NONE', ( #751 ), #21373, .F. ) ;
#1633 = EDGE_CURVE ( 'NONE', #1608, #11692, #15808, .T. ) ;
#1634 = CARTESIAN_POINT ( 'NONE',  ( -16.84758200736127165, 5.154512310753007753, 57.18908790048120494 ) ) ;
#1635 = ORIENTED_EDGE ( 'NONE', *, *, #21786, .T. ) ;
#1636 = DIRECTION ( 'NONE',  ( -0.000000000000000000, -0.000000000000000000, 1.000000000000000000 ) ) ;
#1637 = DIRECTION ( 'NONE',  ( 0.000000000000000000, 1.000000000000000000, 0.000000000000000000 ) ) ;
#1638 = DIRECTION ( 'NONE',  ( -1.000000000000000000, 1.734723475976807834E-16, 0.000000000000000000 ) ) ;
#1639 = CIRCLE ( 'NONE', #14415, 8.999999999999966249 ) ;
#1640 = ADVANCED_FACE ( 'NONE', ( #9117 ), #4496, .F. ) ;
#1641 = CARTESIAN_POINT ( 'NONE',  ( 0.000000000000000000, 7.000000000000000000, 0.000000000000000000 ) ) ;
#1642 = EDGE_CURVE ( 'NONE', #7946, #651, #17286, .T. ) ;
#1643 = ORIENTED_EDGE ( 'NONE', *, *, #4636, .T. ) ;
#1644 = EDGE_CURVE ( 'NONE', #6092, #9113, #22053, .T. ) ;
#1645 = ORIENTED_EDGE ( 'NONE', *, *, #22450, .F. ) ;
#1646 = CLOSED_SHELL ( 'NONE', ( #14748, #6755, #20935, #16987, #10183, #8647, #5905, #22314, #11559, #16889, #11992, #8653 ) ) ;
#1647 = ORIENTED_EDGE ( 'NONE', *, *, #15067, .T. ) ;
#1648 = CARTESIAN_POINT ( 'NONE',  ( 0.000000000000000000, 0.000000000000000000, 0.000000000000000000 ) ) ;
#1649 = ORIENTED_EDGE ( 'NONE', *, *, #7636, .F. ) ;
#1650 = DIRECTION ( 'NONE',  ( 1.296372316667914327E-16, 1.000000000000000000, -0.000000000000000000 ) ) ;
#1651 = AXIS2_PLACEMENT_3D ( 'NONE', #3074, #22337, #8228 ) ;
#1652 = DIRECTION ( 'NONE',  ( -1.000000000000000000, -1.208970125616044077E-17, 0.000000000000000000 ) ) ;
#1653 = DIRECTION ( 'NONE',  ( 0.000000000000000000, 1.000000000000000000, 0.000000000000000000 ) ) ;
#1654 = CARTESIAN_POINT ( 'NONE',  ( 5.967611645685026112, 40.00000000000000000, 52.07955725514904088 ) ) ;
#1655 = ORIENTED_EDGE ( 'NONE', *, *, #6446, .F. ) ;
#1656 = CARTESIAN_POINT ( 'NONE',  ( 11.93972437435558653, 29.14949368109881433, 2.999999999999995559 ) ) ;
#1657 = CARTESIAN_POINT ( 'NONE',  ( 1.110223024625156540E-13, -5.551115123125782702E-14, -6.999999999999950262 ) ) ;
#1658 = ORIENTED_EDGE ( 'NONE', *, *, #14495, .T. ) ;
#1659 = ORIENTED_EDGE ( 'NONE', *, *, #20988, .F. ) ;
#1660 = DIRECTION ( 'NONE',  ( 0.000000000000000000, 0.000000000000000000, -1.000000000000000000 ) ) ;
#1661 = EDGE_LOOP ( 'NONE', ( #6020, #16109, #16262, #15546 ) ) ;
#1662 = PLANE ( 'NONE',  #19986 ) ;
#1663 = AXIS2_PLACEMENT_3D ( 'NONE', #9499, #12798, #435 ) ;
#1664 = CARTESIAN_POINT ( 'NONE',  ( -34.00000000000000000, -6.180736333215561373, 4.163799117101000559E-15 ) ) ;
#1665 = CARTESIAN_POINT ( 'NONE',  ( -0.9019241164162912217, 39.99518131173311986, 49.42300732039321076 ) ) ;
#1666 = DIRECTION ( 'NONE',  ( 0.000000000000000000, 0.000000000000000000, -1.000000000000000000 ) ) ;
#1667 = CARTESIAN_POINT ( 'NONE',  ( -13.00000000000011546, 42.51666049839536043, -105.0010000000000048 ) ) ;
#1668 = EDGE_CURVE ( 'NONE', #19116, #11797, #16440, .T. ) ;
#1669 = CIRCLE ( 'NONE', #3863, 60.00000000000000000 ) ;
#1670 = DIRECTION ( 'NONE',  ( -0.000000000000000000, 1.000000000000000000, -0.000000000000000000 ) ) ;
#1671 = ORIENTED_EDGE ( 'NONE', *, *, #14527, .T. ) ;
#1672 = ORIENTED_EDGE ( 'NONE', *, *, #19117, .T. ) ;
#1673 = EDGE_CURVE ( 'NONE', #16039, #2202, #2606, .T. ) ;
#1674 = ORIENTED_EDGE ( 'NONE', *, *, #1642, .T. ) ;
#1675 = AXIS2_PLACEMENT_3D ( 'NONE', #11723, #4855, #15373 ) ;
#1676 = ORIENTED_EDGE ( 'NONE', *, *, #17223, .F. ) ;
#1677 = CARTESIAN_POINT ( 'NONE',  ( -35.00000000000058265, 26.00000000000000355, -55.00000000000076028 ) ) ;
#1678 = CYLINDRICAL_SURFACE ( 'NONE', #14726, 0.9999999999999974465 ) ;
#1679 = CIRCLE ( 'NONE', #19987, 2.999999999999999112 ) ;
#1680 = DIRECTION ( 'NONE',  ( -0.000000000000000000, -1.000000000000000000, -0.000000000000000000 ) ) ;
#1681 = CARTESIAN_POINT ( 'NONE',  ( 21.66577056626872633, -3.820259908672546167, -2.999999999999971578 ) ) ;
#1682 = VECTOR ( 'NONE', #1745, 1000.000000000000000 ) ;
#1683 = CARTESIAN_POINT ( 'NONE',  ( 0.5415566900166211006, 39.99826507346841709, 49.15084922740629736 ) ) ;
#1684 = AXIS2_PLACEMENT_3D ( 'NONE', #17713, #14492, #2138 ) ;
#1685 = ORIENTED_EDGE ( 'NONE', *, *, #19206, .T. ) ;
#1686 = CARTESIAN_POINT ( 'NONE',  ( -34.09574698892485856, -10.01544929272315088, 3.000000000000056399 ) ) ;
#1687 = CARTESIAN_POINT ( 'NONE',  ( -6.975411493712906363, 39.99999999999999289, -52.53649954156576740 ) ) ;
#1688 = CARTESIAN_POINT ( 'NONE',  ( 1.110223024625156540E-13, -5.551115123125782702E-14, -6.999999999999950262 ) ) ;
#1689 = DIRECTION ( 'NONE',  ( 0.000000000000000000, 1.000000000000000000, 0.000000000000000000 ) ) ;
#1690 = ADVANCED_FACE ( 'NONE', ( #7733 ), #5670, .T. ) ;
#1691 = VERTEX_POINT ( 'NONE', #17698 ) ;
#1692 = PRESENTATION_STYLE_ASSIGNMENT (( #19342 ) ) ;
#1693 = CIRCLE ( 'NONE', #13357, 41.00000000000000000 ) ;
#1694 = ORIENTED_EDGE ( 'NONE', *, *, #22279, .T. ) ;
#1695 = FACE_BOUND ( 'NONE', #20390, .T. ) ;
#1696 = AXIS2_PLACEMENT_3D ( 'NONE', #22355, #2878, #22124 ) ;
#1697 = DIRECTION ( 'NONE',  ( 1.000000000000000000, 0.000000000000000000, 0.000000000000000000 ) ) ;
#1698 = DIRECTION ( 'NONE',  ( 0.000000000000000000, 0.000000000000000000, -1.000000000000000000 ) ) ;
#1699 = CARTESIAN_POINT ( 'NONE',  ( 42.50000000000000711, -12.00000000000000000, -47.50000000000000000 ) ) ;
#1700 = VERTEX_POINT ( 'NONE', #2008 ) ;
#1701 = AXIS2_PLACEMENT_3D ( 'NONE', #19714, #14292, #10986 ) ;
#1702 = VERTEX_POINT ( 'NONE', #285 ) ;
#1703 = ORIENTED_EDGE ( 'NONE', *, *, #17438, .T. ) ;
#1704 =( REPRESENTATION_RELATIONSHIP ('NONE','NONE', #8442, #21292 ) REPRESENTATION_RELATIONSHIP_WITH_TRANSFORMATION ( #13396 )SHAPE_REPRESENTATION_RELATIONSHIP( ) );
#1705 = CARTESIAN_POINT ( 'NONE',  ( 1.522021317812884300, -4.618502324868824616, -46.61386490714788522 ) ) ;
#1706 = CARTESIAN_POINT ( 'NONE',  ( 11.77933723464115445, 40.00000000000000000, -54.24924979334851116 ) ) ;
#1707 = EDGE_LOOP ( 'NONE', ( #708, #14419, #2679, #4198, #18260, #21957, #20036, #20335 ) ) ;
#1708 = EDGE_CURVE ( 'NONE', #19434, #18082, #21683, .T. ) ;
#1709 = CARTESIAN_POINT ( 'NONE',  ( 1.110223024625156540E-13, -5.551115123125782702E-14, -6.999999999999950262 ) ) ;
#1710 = LINE ( 'NONE', #16802, #7044 ) ;
#1711 = LINE ( 'NONE', #14047, #14166 ) ;
#1712 = CARTESIAN_POINT ( 'NONE',  ( -17.18568680885986666, 30.37812028685642218, -59.88587632368449221 ) ) ;
#1713 = FACE_OUTER_BOUND ( 'NONE', #5783, .T. ) ;
#1714 = EDGE_CURVE ( 'NONE', #12526, #19349, #10771, .T. ) ;
#1715 = AXIS2_PLACEMENT_3D ( 'NONE', #7984, #21973, #12889 ) ;
#1716 = ORIENTED_EDGE ( 'NONE', *, *, #18989, .F. ) ;
#1717 = DIRECTION ( 'NONE',  ( 0.000000000000000000, 1.000000000000000000, 0.000000000000000000 ) ) ;
#1718 = DIRECTION ( 'NONE',  ( -0.000000000000000000, 1.000000000000000000, -0.000000000000000000 ) ) ;
#1719 = LINE ( 'NONE', #21188, #13756 ) ;
#1720 = CARTESIAN_POINT ( 'NONE',  ( -36.54278193890294091, -4.025500340002652777, 2.800654218530481465 ) ) ;
#1721 = ORIENTED_EDGE ( 'NONE', *, *, #14368, .F. ) ;
#1722 = CARTESIAN_POINT ( 'NONE',  ( 35.00000000000000000, 2.142135623730931471, 4.258610482196280173E-15 ) ) ;
#1723 = CARTESIAN_POINT ( 'NONE',  ( -42.50000000000000711, -12.00000000000012434, -44.97499999999988773 ) ) ;
#1724 = AXIS2_PLACEMENT_3D ( 'NONE', #15557, #93, #5162 ) ;
#1725 = EDGE_CURVE ( 'NONE', #2966, #11042, #17270, .T. ) ;
#1726 = ORIENTED_EDGE ( 'NONE', *, *, #10016, .F. ) ;
#1727 = PRODUCT_CONTEXT ( 'NONE', #18977, 'mechanical' ) ;
#1728 = EDGE_CURVE ( 'NONE', #11390, #6332, #7045, .T. ) ;
#1729 = VERTEX_POINT ( 'NONE', #18275 ) ;
#1730 = DIRECTION ( 'NONE',  ( 0.000000000000000000, 1.000000000000000000, 0.000000000000000000 ) ) ;
#1731 = CARTESIAN_POINT ( 'NONE',  ( 8.349099696861289388, 1.803277857259551364, -53.93591755799868537 ) ) ;
#1732 = AXIS2_PLACEMENT_3D ( 'NONE', #22641, #3717, #20676 ) ;
#1733 = FACE_OUTER_BOUND ( 'NONE', #6732, .T. ) ;
#1734 = CARTESIAN_POINT ( 'NONE',  ( 4.936596639065371050, 31.11077005834392395, -2.999999999999975131 ) ) ;
#1735 = CARTESIAN_POINT ( 'NONE',  ( 22.12933039895921894, 3.000000000000003109, 3.436930240568481542E-15 ) ) ;
#1736 = VECTOR ( 'NONE', #9880, 1000.000000000000000 ) ;
#1737 = VERTEX_POINT ( 'NONE', #20454 ) ;
#1738 = FACE_OUTER_BOUND ( 'NONE', #22008, .T. ) ;
#1739 = CARTESIAN_POINT ( 'NONE',  ( -11.03199507241031618, 40.00000000000000000, -53.98106524768372338 ) ) ;
#1740 = ORIENTED_EDGE ( 'NONE', *, *, #9652, .F. ) ;
#1741 = DIRECTION ( 'NONE',  ( 0.000000000000000000, 1.000000000000000000, 0.000000000000000000 ) ) ;
#1742 = CIRCLE ( 'NONE', #2089, 3.000000000000002665 ) ;
#1743 = CARTESIAN_POINT ( 'NONE',  ( 20.15166188517204304, 29.89072699358925433, -58.13409936646343823 ) ) ;
#1744 = LINE ( 'NONE', #12270, #4214 ) ;
#1745 = DIRECTION ( 'NONE',  ( 1.296372316667914327E-16, 1.000000000000000000, -0.000000000000000000 ) ) ;
#1746 = CARTESIAN_POINT ( 'NONE',  ( -6.631891324090021023, 39.71688158846335881, -53.15285336691422202 ) ) ;
#1747 = ORIENTED_EDGE ( 'NONE', *, *, #6797, .T. ) ;
#1748 = CARTESIAN_POINT ( 'NONE',  ( 20.00000000000004974, -2.506448799221099482E-14, 2.999999999999995559 ) ) ;
#1749 = ADVANCED_FACE ( 'NONE', ( #4646 ), #4530, .F. ) ;
#1750 = DIRECTION ( 'NONE',  ( 1.049727191138618326E-16, -0.5150380749100547106, 0.8571673007021120005 ) ) ;
#1751 = VERTEX_POINT ( 'NONE', #11392 ) ;
#1752 = CARTESIAN_POINT ( 'NONE',  ( 11.68987541775893391, 3.735186999536483921, 55.40064774187846552 ) ) ;
#1753 = VECTOR ( 'NONE', #17415, 1000.000000000000000 ) ;
#1754 = AXIS2_PLACEMENT_3D ( 'NONE', #3712, #21577, #721 ) ;
#1755 = DIRECTION ( 'NONE',  ( 0.1421319796954317316, 0.000000000000000000, 0.9898477157360405787 ) ) ;
#1756 = FACE_OUTER_BOUND ( 'NONE', #13620, .T. ) ;
#1757 = AXIS2_PLACEMENT_3D ( 'NONE', #9404, #14192, #10999 ) ;
#1758 = ADVANCED_FACE ( 'NONE', ( #2585 ), #3762, .F. ) ;
#1759 = AXIS2_PLACEMENT_3D ( 'NONE', #7535, #9704, #14727 ) ;
#1760 = ORIENTED_EDGE ( 'NONE', *, *, #4883, .T. ) ;
#1761 = ORIENTED_EDGE ( 'NONE', *, *, #17671, .T. ) ;
#1762 = ORIENTED_EDGE ( 'NONE', *, *, #19139, .T. ) ;
#1764 = ADVANCED_FACE ( 'NONE', ( #11512 ), #16551, .T. ) ;
#1763 =( LENGTH_UNIT ( ) NAMED_UNIT ( * ) SI_UNIT ( .MILLI., .METRE. ) );
#1765 = EDGE_CURVE ( 'NONE', #17743, #6038, #8882, .T. ) ;
#1766 = EDGE_CURVE ( 'NONE', #1817, #14184, #21715, .T. ) ;
#1767 = VERTEX_POINT ( 'NONE', #11621 ) ;
#1768 = CARTESIAN_POINT ( 'NONE',  ( 0.000000000000000000, 30.00000000000000000, 0.000000000000000000 ) ) ;
#1769 = CARTESIAN_POINT ( 'NONE',  ( 2.220446049250313081E-13, -2.498001805406602216E-13, -6.859353255829918616 ) ) ;
#1770 = CARTESIAN_POINT ( 'NONE',  ( 2.274190170887435691, 40.00000000000000000, 50.13372671147816106 ) ) ;
#1771 = AXIS2_PLACEMENT_3D ( 'NONE', #8287, #15255, #22277 ) ;
#1772 = ORIENTED_EDGE ( 'NONE', *, *, #12359, .F. ) ;
#1773 = DIRECTION ( 'NONE',  ( 0.000000000000000000, 0.000000000000000000, 1.000000000000000000 ) ) ;
#1774 = CARTESIAN_POINT ( 'NONE',  ( -1.522021317825201336, -4.618502324872293840, -46.61386490715217690 ) ) ;
#1775 = ORIENTED_EDGE ( 'NONE', *, *, #13470, .T. ) ;
#1776 = CYLINDRICAL_SURFACE ( 'NONE', #3534, 17.00000000000000711 ) ;
#1777 = CIRCLE ( 'NONE', #12365, 2.099999999999997868 ) ;
#1778 = VECTOR ( 'NONE', #2503, 1000.000000000000000 ) ;
#1779 = DIRECTION ( 'NONE',  ( 1.000000000000000000, 1.208970125616053321E-17, 0.000000000000000000 ) ) ;
#1780 = ORIENTED_EDGE ( 'NONE', *, *, #6189, .T. ) ;
#1781 = CARTESIAN_POINT ( 'NONE',  ( 0.000000000000000000, 30.00000000000000000, 0.000000000000000000 ) ) ;
#1782 = AXIS2_PLACEMENT_3D ( 'NONE', #12775, #6026, #14609 ) ;
#1783 = EDGE_CURVE ( 'NONE', #10281, #4282, #12160, .T. ) ;
#1784 = DIRECTION ( 'NONE',  ( -1.000000000000000000, -5.354846555474805578E-15, 0.000000000000000000 ) ) ;
#1785 = AXIS2_PLACEMENT_3D ( 'NONE', #18466, #4737, #18248 ) ;
#1786 = CARTESIAN_POINT ( 'NONE',  ( -4.586067100669611207, 39.86904425122069995, 51.95541839444461374 ) ) ;
#1787 = CARTESIAN_POINT ( 'NONE',  ( 22.29034605647553136, 17.39518641927312714, 58.63862881473038158 ) ) ;
#1788 = CARTESIAN_POINT ( 'NONE',  ( -2.467804172277818612E-14, 1.500000000000002887, 11.99999999999966960 ) ) ;
#1789 = FACE_OUTER_BOUND ( 'NONE', #2176, .T. ) ;
#1790 = AXIS2_PLACEMENT_3D ( 'NONE', #4562, #17989, #11540 ) ;
#1791 = AXIS2_PLACEMENT_3D ( 'NONE', #4033, #12375, #113 ) ;
#1792 = ORIENTED_EDGE ( 'NONE', *, *, #7408, .T. ) ;
#1793 = AXIS2_PLACEMENT_3D ( 'NONE', #5535, #12510, #17457 ) ;
#1794 = VERTEX_POINT ( 'NONE', #6132 ) ;
#1795 = VERTEX_POINT ( 'NONE', #4419 ) ;
#1796 = ORIENTED_EDGE ( 'NONE', *, *, #2744, .F. ) ;
#1797 = DIRECTION ( 'NONE',  ( 1.296372316667914327E-16, 1.000000000000000000, -0.000000000000000000 ) ) ;
#1798 = DIRECTION ( 'NONE',  ( 6.505213034913038160E-19, 3.903127820947822896E-18, 1.000000000000000000 ) ) ;
#1799 = PRODUCT ( 'MAS-345', 'MAS-345', '', ( #4938 ) ) ;
#1800 = DIRECTION ( 'NONE',  ( -1.000000000000000000, -1.208970125616046080E-17, 6.505213034913038160E-19 ) ) ;
#1801 = CARTESIAN_POINT ( 'NONE',  ( 0.05198799887590952601, 39.99998426521146655, 48.77440217005271705 ) ) ;
#1802 = EDGE_CURVE ( 'NONE', #7505, #5679, #9677, .T. ) ;
#1803 = EDGE_CURVE ( 'NONE', #13632, #20362, #5094, .T. ) ;
#1804 = CIRCLE ( 'NONE', #9122, 2.499999999999998668 ) ;
#1805 = ORIENTED_EDGE ( 'NONE', *, *, #12333, .F. ) ;
#1806 = DIRECTION ( 'NONE',  ( -0.000000000000000000, 1.000000000000000000, -0.000000000000000000 ) ) ;
#1807 = DIRECTION ( 'NONE',  ( 0.000000000000000000, 0.000000000000000000, -1.000000000000000000 ) ) ;
#1808 = CARTESIAN_POINT ( 'NONE',  ( -22.12933039895921183, 3.000000000000009326, 0.000000000000000000 ) ) ;
#1809 = CARTESIAN_POINT ( 'NONE',  ( 27.01645732367857633, 17.86915608785674792, 3.000000000000023537 ) ) ;
#1810 = EDGE_CURVE ( 'NONE', #10947, #5838, #8753, .T. ) ;
#1811 = FILL_AREA_STYLE_COLOUR ( '', #19401 ) ;
#1812 = DIRECTION ( 'NONE',  ( 1.000000000000000000, 0.000000000000000000, 0.000000000000000000 ) ) ;
#1813 = FACE_BOUND ( 'NONE', #15683, .T. ) ;
#1814 = DIRECTION ( 'NONE',  ( 0.000000000000000000, -0.000000000000000000, 1.000000000000000000 ) ) ;
#1815 = CARTESIAN_POINT ( 'NONE',  ( -1.387778780781445518E-14, 20.00000000000000355, -105.0000000000000142 ) ) ;
#1816 = B_SPLINE_CURVE_WITH_KNOTS ( 'NONE', 3,
 ( #7333, #10873, #9054, #14418, #7217, #2178 ),
 .UNSPECIFIED., .F., .F.,
 ( 4, 2, 4 ),
 ( 1.845645724737087379E-18, 0.002694896630591183447, 0.005389793261182365160 ),
 .UNSPECIFIED. ) ;
#1817 = VERTEX_POINT ( 'NONE', #12074 ) ;
#1818 = EDGE_LOOP ( 'NONE', ( #1300, #6762, #10355, #11585 ) ) ;
#1819 = CIRCLE ( 'NONE', #19020, 19.11328065563150957 ) ;
#1820 = ORIENTED_EDGE ( 'NONE', *, *, #13645, .F. ) ;
#1821 = CARTESIAN_POINT ( 'NONE',  ( 42.49999999999998579, 10.00000000000000000, -53.99999999999997868 ) ) ;
#1822 = CARTESIAN_POINT ( 'NONE',  ( 2.775557561562891351E-14, -2.775557561562891351E-14, 2.999999999999995559 ) ) ;
#1823 = VERTEX_POINT ( 'NONE', #15269 ) ;
#1824 = CARTESIAN_POINT ( 'NONE',  ( 3.469446951953614189E-15, 38.23275711891355400, 0.000000000000000000 ) ) ;
#1825 =( BOUNDED_SURFACE ( )  B_SPLINE_SURFACE ( 3, 2, ( 
 ( #151, #4068, #9325 ),
 ( #14693, #8066, #1077 ),
 ( #21937, #19869, #4291 ),
 ( #2457, #16302, #4404 ),
 ( #11263, #9551, #21701 ),
 ( #6231, #13191, #4172 ),
 ( #19762, #9443, #615 ),
 ( #21470, #12751, #7719 ),
 ( #11148, #16536, #14802 ),
 ( #11035, #839, #19982 ),
 ( #7950, #18142, #5889 ),
 ( #12857, #7829, #20098 ),
 ( #16423, #21817, #738 ),
 ( #5998, #6116, #13079 ) ),
 .UNSPECIFIED., .F., .F., .F. ) 
 B_SPLINE_SURFACE_WITH_KNOTS ( ( 4, 2, 2, 2, 2, 2, 4 ),
 ( 3, 3 ),
 ( 0.004259382447192771454, 0.005809352080732710713, 0.007359321714272649105, 0.008909291347812587497, 0.01045926098135252676, 0.01355920024843240354, 0.01665913951551228206 ),
 ( 0.000000000000000000, 0.8363185636274830248 ),
 .UNSPECIFIED. ) 
 GEOMETRIC_REPRESENTATION_ITEM ( )  RATIONAL_B_SPLINE_SURFACE ( (
 ( 1.000000000000000000, 0.7012747261256253584, 0.9022084361829376675),
 ( 1.000000000000000000, 0.7322972190981885676, 0.9123640486021487028),
 ( 1.000000000000000000, 0.7591999772719525419, 0.9211710128026768807),
 ( 1.000000000000000000, 0.8072870422117247591, 0.9369129325232377070),
 ( 1.000000000000000000, 0.8284615345039458845, 0.9438446751489368847),
 ( 1.000000000000000000, 0.8663823161282082630, 0.9562585311581923708),
 ( 1.000000000000000000, 0.8831521068476495540, 0.9617483380234417290),
 ( 1.000000000000000000, 0.9127686518824577044, 0.9714436952868192865),
 ( 1.000000000000000000, 0.9255811113611541741, 0.9756380188286946087),
 ( 1.000000000000000000, 0.9589863376200309375, 0.9865736496614985196),
 ( 1.000000000000000000, 0.9746016745770703649, 0.9916855312266366074),
 ( 1.000000000000000000, 0.9951270285874161958, 0.9984047700795721791),
 ( 1.000000000000000000, 0.9999818007053916658, 0.9999940422266351270),
 ( 1.000000000000000000, 1.000000000000000000, 1.000000000000000000) ) ) 
 REPRESENTATION_ITEM ( '' )  SURFACE ( )  );
#1826 = CARTESIAN_POINT ( 'NONE',  ( 28.45046755804883531, -15.62726112422599378, -2.999999999999971578 ) ) ;
#1827 = DIRECTION ( 'NONE',  ( 6.505213034913038160E-19, 3.903127820947822896E-18, 1.000000000000000000 ) ) ;
#1828 = CARTESIAN_POINT ( 'NONE',  ( -10.55176496409658604, 37.02956028564889124, -54.80914071361400630 ) ) ;
#1829 = CYLINDRICAL_SURFACE ( 'NONE', #7148, 0.9999999999999974465 ) ;
#1830 = CIRCLE ( 'NONE', #4408, 19.11328065563152379 ) ;
#1831 = ORIENTED_EDGE ( 'NONE', *, *, #22079, .F. ) ;
#1832 = DIRECTION ( 'NONE',  ( -1.000000000000000000, -1.208970125616044077E-17, 0.000000000000000000 ) ) ;
#1833 = SURFACE_STYLE_FILL_AREA ( #3558 ) ;
#1834 = FACE_OUTER_BOUND ( 'NONE', #6477, .T. ) ;
#1835 = CARTESIAN_POINT ( 'NONE',  ( 34.88850421923977763, -1.128083539116253586, 3.000000000000023537 ) ) ;
#1836 = ORIENTED_EDGE ( 'NONE', *, *, #8521, .F. ) ;
#1837 = CARTESIAN_POINT ( 'NONE',  ( 36.54278193890314697, 4.025500340002402311, -2.800654218530457484 ) ) ;
#1838 = CARTESIAN_POINT ( 'NONE',  ( -35.00000000000000000, -9.000000000000001776, 14.00000000000001421 ) ) ;
#1839 = EDGE_CURVE ( 'NONE', #3030, #17217, #20670, .T. ) ;
#1840 = EDGE_LOOP ( 'NONE', ( #9020, #7436, #19859 ) ) ;
#1841 = ADVANCED_FACE ( 'NONE', ( #10229 ), #21011, .T. ) ;
#1842 = VERTEX_POINT ( 'NONE', #17221 ) ;
#1843 = CARTESIAN_POINT ( 'NONE',  ( 2.999999999999998668, 22.79878727884707956, 6.485281374238567764 ) ) ;
#1844 = CARTESIAN_POINT ( 'NONE',  ( -35.00000000000000000, -15.00000000000000000, 15.00000000000002132 ) ) ;
#1845 = FACE_OUTER_BOUND ( 'NONE', #19525, .T. ) ;
#1846 = CARTESIAN_POINT ( 'NONE',  ( 2.775557561562891351E-14, 2.775557561562891351E-14, 5.750000000000001776 ) ) ;
#1847 = CARTESIAN_POINT ( 'NONE',  ( 25.99999999999998579, 19.99999999999999645, 105.0000000000000142 ) ) ;
#1848 = ORIENTED_EDGE ( 'NONE', *, *, #7591, .T. ) ;
#1849 = CARTESIAN_POINT ( 'NONE',  ( -25.00000000000000000, 20.00000000000000000, 6.487780019669002523E-15 ) ) ;
#1850 = CARTESIAN_POINT ( 'NONE',  ( 42.50000000000000711, -9.600000000000001421, -49.60000000000000142 ) ) ;
#1851 = ORIENTED_EDGE ( 'NONE', *, *, #3289, .F. ) ;
#1852 = DIRECTION ( 'NONE',  ( 1.445602896647339410E-16, 0.000000000000000000, 1.000000000000000000 ) ) ;
#1853 = CARTESIAN_POINT ( 'NONE',  ( -34.99999999999999289, -5.000000000000000000, 4.999999999999969802 ) ) ;
#1855 = AXIS2_PLACEMENT_3D ( 'NONE', #2978, #3205, #13487 ) ;
#1854 = FACE_OUTER_BOUND ( 'NONE', #17768, .T. ) ;
#1856 = CARTESIAN_POINT ( 'NONE',  ( -4.996179737156035472, 39.84467275235065387, -52.21079479358778741 ) ) ;
#1857 = ORIENTED_EDGE ( 'NONE', *, *, #4842, .T. ) ;
#1858 = LINE ( 'NONE', #7117, #6849 ) ;
#1859 = CARTESIAN_POINT ( 'NONE',  ( -20.34735785252017237, 29.47800210776924601, 58.18363580933387880 ) ) ;
#1860 = CARTESIAN_POINT ( 'NONE',  ( 11.00126833624750766, 3.276569432396202242, 57.62199738689401585 ) ) ;
#1861 = CYLINDRICAL_SURFACE ( 'NONE', #185, 17.00000000000000000 ) ;
#1862 = CARTESIAN_POINT ( 'NONE',  ( -34.99999999999980815, 40.00000000000000000, 54.99999999999922551 ) ) ;
#1863 = ADVANCED_FACE ( 'NONE', ( #6926 ), #16193, .T. ) ;
#1864 = AXIS2_PLACEMENT_3D ( 'NONE', #7257, #15830, #142 ) ;
#1865 = ORIENTED_EDGE ( 'NONE', *, *, #5944, .F. ) ;
#1866 = EDGE_CURVE ( 'NONE', #18033, #8806, #17562, .T. ) ;
#1867 = AXIS2_PLACEMENT_3D ( 'NONE', #14446, #11021, #16064 ) ;
#1868 = ORIENTED_EDGE ( 'NONE', *, *, #15920, .F. ) ;
#1869 = VERTEX_POINT ( 'NONE', #4975 ) ;
#1870 = ORIENTED_EDGE ( 'NONE', *, *, #10684, .F. ) ;
#1871 = CARTESIAN_POINT ( 'NONE',  ( -8.646032897229122938, 31.21605069118058040, -6.999999999999950262 ) ) ;
#1872 = CARTESIAN_POINT ( 'NONE',  ( 18.49252681899428197, 7.260825773989753706, 57.68517796515787666 ) ) ;
#1873 = CARTESIAN_POINT ( 'NONE',  ( 9.505538832396775106, 39.99999999999999289, -53.50900172497617291 ) ) ;
#1874 = CARTESIAN_POINT ( 'NONE',  ( 7.313763269676020862, 40.00000000000000711, 52.68151666842681635 ) ) ;
#1875 = VERTEX_POINT ( 'NONE', #3145 ) ;
#1876 = CARTESIAN_POINT ( 'NONE',  ( -35.00000000000000000, 39.00000000000000711, 1.387778780781445676E-14 ) ) ;
#1877 = CARTESIAN_POINT ( 'NONE',  ( -0.7217013448959017641, -4.626342591392887726, -46.01887142923196450 ) ) ;
#1878 = ORIENTED_EDGE ( 'NONE', *, *, #9036, .T. ) ;
#1879 = CYLINDRICAL_SURFACE ( 'NONE', #4631, 2.099999999999997868 ) ;
#1880 = CIRCLE ( 'NONE', #5533, 1.000000000000001776 ) ;
#1881 = DIRECTION ( 'NONE',  ( -0.000000000000000000, -1.000000000000000000, -0.000000000000000000 ) ) ;
#1882 = ORIENTED_EDGE ( 'NONE', *, *, #8202, .F. ) ;
#1883 = ADVANCED_FACE ( 'NONE', ( #3605 ), #9242, .T. ) ;
#1884 = CARTESIAN_POINT ( 'NONE',  ( -90.00000000000000000, 28.00000000000000000, -2.500000000000003109 ) ) ;
#1885 = ORIENTED_EDGE ( 'NONE', *, *, #3594, .F. ) ;
#1886 = CARTESIAN_POINT ( 'NONE',  ( 35.43002037646326841, -7.196011215416819873, -2.933296326616337435 ) ) ;
#1887 = DIRECTION ( 'NONE',  ( -0.000000000000000000, -1.000000000000000000, -0.000000000000000000 ) ) ;
#1888 = CARTESIAN_POINT ( 'NONE',  ( -3.946564738182986698, 39.90443716068799063, 51.55060801955053762 ) ) ;
#1889 = CARTESIAN_POINT ( 'NONE',  ( 19.42347305479415454, 31.41593231561366650, 57.95407386126545646 ) ) ;
#1890 = CARTESIAN_POINT ( 'NONE',  ( 42.50000000000000711, -12.00000000000012434, -44.97499999999988773 ) ) ;
#1891 = ADVANCED_FACE ( 'NONE', ( #10334, #3487 ), #6584, .T. ) ;
#1892 = EDGE_CURVE ( 'NONE', #8190, #7904, #20239, .T. ) ;
#1893 = DIRECTION ( 'NONE',  ( 0.000000000000000000, 0.000000000000000000, 1.000000000000000000 ) ) ;
#1894 = VERTEX_POINT ( 'NONE', #10114 ) ;
#1895 = AXIS2_PLACEMENT_3D ( 'NONE', #17411, #3457, #6656 ) ;
#1896 = ORIENTED_EDGE ( 'NONE', *, *, #13510, .T. ) ;
#1897 = EDGE_CURVE ( 'NONE', #16909, #2243, #3406, .T. ) ;
#1898 = ORIENTED_EDGE ( 'NONE', *, *, #11064, .F. ) ;
#1899 = EDGE_LOOP ( 'NONE', ( #18124, #14504, #19988, #8484 ) ) ;
#1900 = CARTESIAN_POINT ( 'NONE',  ( -31.67162468655987340, -14.67611967928944594, -2.999999999999971578 ) ) ;
#1901 = LINE ( 'NONE', #8880, #1214 ) ;
#1902 = ADVANCED_FACE ( 'NONE', ( #11839 ), #12486, .T. ) ;
#1903 = DIRECTION ( 'NONE',  ( 8.659560562354932858E-17, 0.7071067811865474617, -0.7071067811865474617 ) ) ;
#1904 = CARTESIAN_POINT ( 'NONE',  ( 6.264962364260838967, 39.74816733111172340, 52.94809029108233744 ) ) ;
#1905 = EDGE_CURVE ( 'NONE', #3795, #8449, #2994, .T. ) ;
#1906 = EDGE_LOOP ( 'NONE', ( #11289, #11944, #13198, #17080 ) ) ;
#1907 = DIRECTION ( 'NONE',  ( 1.000000000000000000, 1.208970125616067650E-17, 0.000000000000000000 ) ) ;
#1908 = DIRECTION ( 'NONE',  ( -1.000000000000000000, -1.208970125616060717E-17, 0.000000000000000000 ) ) ;
#1909 = CARTESIAN_POINT ( 'NONE',  ( -25.00000000000000000, -20.00000000000000000, 6.487780019669002523E-15 ) ) ;
#1910 = DIRECTION ( 'NONE',  ( 0.000000000000000000, 1.000000000000000000, 0.000000000000000000 ) ) ;
#1911 = CARTESIAN_POINT ( 'NONE',  ( -16.66666666666665719, 20.00000000000000000, 23.57022603955159923 ) ) ;
#1912 = AXIS2_PLACEMENT_3D ( 'NONE', #1557, #15854, #22421 ) ;
#1913 = CARTESIAN_POINT ( 'NONE',  ( -42.50000000000000711, -12.00000000000000000, 45.00000000000000711 ) ) ;
#1914 = DIRECTION ( 'NONE',  ( 1.000000000000000000, 0.000000000000000000, 0.000000000000000000 ) ) ;
#1915 = CARTESIAN_POINT ( 'NONE',  ( -30.98879172160200213, 17.38064605515573291, 3.000000000000043077 ) ) ;
#1916 = CARTESIAN_POINT ( 'NONE',  ( -24.10117729468380077, 26.10603996529630777, 3.000000000000042188 ) ) ;
#1917 = EDGE_CURVE ( 'NONE', #4478, #16652, #11956, .T. ) ;
#1918 = ORIENTED_EDGE ( 'NONE', *, *, #10579, .T. ) ;
#1919 = ORIENTED_EDGE ( 'NONE', *, *, #19990, .F. ) ;
#1920 = ORIENTED_EDGE ( 'NONE', *, *, #1155, .F. ) ;
#1921 = VECTOR ( 'NONE', #2869, 1000.000000000000000 ) ;
#1922 = CARTESIAN_POINT ( 'NONE',  ( 7.682546357471700560, -2.941798577943465443, -52.37062424970318375 ) ) ;
#1923 = AXIS2_PLACEMENT_3D ( 'NONE', #18496, #11280, #15037 ) ;
#1924 = CARTESIAN_POINT ( 'NONE',  ( 12.01755860117725661, 39.99999999999998579, -54.34185968360765173 ) ) ;
#1925 = AXIS2_PLACEMENT_3D ( 'NONE', #4573, #11549, #2853 ) ;
#1926 = CARTESIAN_POINT ( 'NONE',  ( 28.07080038625117524, 14.29266125237876928, 2.999999999999995559 ) ) ;
#1927 = CARTESIAN_POINT ( 'NONE',  ( 35.00000000000000000, -9.000000000000001776, 9.000000000000007105 ) ) ;
#1928 = CARTESIAN_POINT ( 'NONE',  ( -19.04641992693179020, 13.69305383064222781, 60.38882653684734692 ) ) ;
#1929 = FACE_OUTER_BOUND ( 'NONE', #11415, .T. ) ;
#1930 = CARTESIAN_POINT ( 'NONE',  ( -35.00000000000000000, 14.00000000000000000, 2.365113165210053967E-14 ) ) ;
#1931 = VERTEX_POINT ( 'NONE', #22513 ) ;
#1932 = DIRECTION ( 'NONE',  ( 0.000000000000000000, 1.000000000000000000, 0.000000000000000000 ) ) ;
#1933 = FACE_OUTER_BOUND ( 'NONE', #18238, .T. ) ;
#1934 = CARTESIAN_POINT ( 'NONE',  ( 41.39271818392636959, 10.00000000000000000, -5.943569790512535533 ) ) ;
#1935 = CARTESIAN_POINT ( 'NONE',  ( 0.000000000000000000, -40.00000000000000000, 5.000000000000000000 ) ) ;
#1936 = ORIENTED_EDGE ( 'NONE', *, *, #18548, .F. ) ;
#1937 = AXIS2_PLACEMENT_3D ( 'NONE', #10361, #1558, #17361 ) ;
#1938 = LINE ( 'NONE', #13847, #10442 ) ;
#1939 = CARTESIAN_POINT ( 'NONE',  ( -34.99999999999980815, 39.97500000000000142, 57.49999999999921840 ) ) ;
#1940 = AXIS2_PLACEMENT_3D ( 'NONE', #21222, #19502, #19846 ) ;
#1941 = EDGE_CURVE ( 'NONE', #16162, #12420, #4452, .T. ) ;
#1942 = EDGE_LOOP ( 'NONE', ( #18055, #2733, #2323, #16683 ) ) ;
#1943 = ADVANCED_FACE ( 'NONE', ( #2316 ), #479, .F. ) ;
#1944 = ORIENTED_EDGE ( 'NONE', *, *, #1708, .F. ) ;
#1945 = CARTESIAN_POINT ( 'NONE',  ( 2.999999999999998668, 22.79878727884707956, 8.485281374238567764 ) ) ;
#1946 = DIRECTION ( 'NONE',  ( 0.000000000000000000, 0.000000000000000000, 1.000000000000000000 ) ) ;
#1947 = TOROIDAL_SURFACE ( 'NONE', #3788, 34.90673715956759082, 8.750000000000000000 ) ;
#1948 = CARTESIAN_POINT ( 'NONE',  ( -8.215393105055655454, 1.749144060402859857, 56.08634520686069180 ) ) ;
#1949 = CARTESIAN_POINT ( 'NONE',  ( 35.00000000000000000, -15.00000000000000000, 2.255140518769849223E-14 ) ) ;
#1950 = ORIENTED_EDGE ( 'NONE', *, *, #10208, .F. ) ;
#1951 = FACE_BOUND ( 'NONE', #22385, .T. ) ;
#1952 = AXIS2_PLACEMENT_3D ( 'NONE', #9959, #4929, #22467 ) ;
#1953 = CARTESIAN_POINT ( 'NONE',  ( -7.349635197212319504, 40.00000000000000000, 52.69668167434164729 ) ) ;
#1954 = EDGE_LOOP ( 'NONE', ( #15619, #232 ) ) ;
#1955 = FACE_OUTER_BOUND ( 'NONE', #1270, .T. ) ;
#1956 = AXIS2_PLACEMENT_3D ( 'NONE', #9749, #21909, #4488 ) ;
#1957 = EDGE_CURVE ( 'NONE', #12666, #15098, #19511, .T. ) ;
#1958 = CARTESIAN_POINT ( 'NONE',  ( 2.775557561562891351E-14, 2.775557561562891351E-14, 5.750000000000001776 ) ) ;
#1959 = DIRECTION ( 'NONE',  ( 1.000000000000000000, 0.000000000000000000, 0.000000000000000000 ) ) ;
#1960 = CARTESIAN_POINT ( 'NONE',  ( 0.000000000000000000, 30.00000000000000355, 0.000000000000000000 ) ) ;
#1961 = ORIENTED_EDGE ( 'NONE', *, *, #21275, .T. ) ;
#1962 = DIRECTION ( 'NONE',  ( 0.000000000000000000, 0.000000000000000000, 1.000000000000000000 ) ) ;
#1963 = CARTESIAN_POINT ( 'NONE',  ( -12.27586057105632378, 4.193657236093761398, 55.54740530681011990 ) ) ;
#1964 = CARTESIAN_POINT ( 'NONE',  ( -8.230913598554863597, 39.55470085923248291, -53.98103024247675563 ) ) ;
#1965 = ORIENTED_EDGE ( 'NONE', *, *, #9711, .F. ) ;
#1966 = ADVANCED_FACE ( 'NONE', ( #10780 ), #2206, .F. ) ;
#1967 = AXIS2_PLACEMENT_3D ( 'NONE', #22562, #6856, #13822 ) ;
#1968 = CARTESIAN_POINT ( 'NONE',  ( 3.330669073875469621E-13, -1.110223024625156540E-13, -2.999999999999971578 ) ) ;
#1969 = FACE_OUTER_BOUND ( 'NONE', #15934, .T. ) ;
#1970 = CIRCLE ( 'NONE', #3085, 4.999999999999997335 ) ;
#1971 = AXIS2_PLACEMENT_3D ( 'NONE', #21641, #673, #21759 ) ;
#1972 = AXIS2_PLACEMENT_3D ( 'NONE', #8588, #18795, #6882 ) ;
#1973 = ORIENTED_EDGE ( 'NONE', *, *, #11285, .F. ) ;
#1974 = EDGE_LOOP ( 'NONE', ( #17985, #19237, #10620, #7582 ) ) ;
#1975 = ORIENTED_EDGE ( 'NONE', *, *, #2118, .T. ) ;
#1976 = SHAPE_REPRESENTATION_RELATIONSHIP ( 'NONE' , 'NONE' ,  #18960, #19467 ) ;
#1977 = EDGE_LOOP ( 'NONE', ( #11008, #9081 ) ) ;
#1978 = FACE_OUTER_BOUND ( 'NONE', #2696, .T. ) ;
#1979 = DIRECTION ( 'NONE',  ( 0.000000000000000000, 0.000000000000000000, 1.000000000000000000 ) ) ;
#1980 = CARTESIAN_POINT ( 'NONE',  ( 6.629170412548176294, 39.71713055914890589, -53.15137697417961959 ) ) ;
#1981 = CARTESIAN_POINT ( 'NONE',  ( 5.030996208853185436, 39.99999999999998579, 51.62610378409378598 ) ) ;
#1982 = EDGE_LOOP ( 'NONE', ( #8822, #16245, #2807, #12860 ) ) ;
#1983 = DIRECTION ( 'NONE',  ( -6.505213034913038160E-19, -3.903127820947822896E-18, -1.000000000000000000 ) ) ;
#1984 = CARTESIAN_POINT ( 'NONE',  ( 0.1963897509099326311, -3.154216256267534213, -47.17168727993868060 ) ) ;
#1985 = VERTEX_POINT ( 'NONE', #12497 ) ;
#1986 = LINE ( 'NONE', #16071, #20757 ) ;
#1987 = EDGE_CURVE ( 'NONE', #9166, #6590, #21289, .T. ) ;
#1988 = CARTESIAN_POINT ( 'NONE',  ( -4.295527433237782828E-15, -1.236374842841486021, 48.24164917503448180 ) ) ;
#1989 = VECTOR ( 'NONE', #13933, 1000.000000000000000 ) ;
#1990 = CARTESIAN_POINT ( 'NONE',  ( 15.49999999999993783, 42.51666049839543149, -105.0010000000000048 ) ) ;
#1991 = ORIENTED_EDGE ( 'NONE', *, *, #15486, .T. ) ;
#1992 = CARTESIAN_POINT ( 'NONE',  ( 6.696867368502865039E-15, 35.00000000000000000, 38.73397172404480671 ) ) ;
#1993 = ORIENTED_EDGE ( 'NONE', *, *, #14587, .T. ) ;
#1994 = CARTESIAN_POINT ( 'NONE',  ( -2.999999999999998668, 22.00000000000000355, 6.485281374238567764 ) ) ;
#1995 = CARTESIAN_POINT ( 'NONE',  ( -4.240361389880785481, 39.54844917561619866, 53.29842195655543691 ) ) ;
#1996 = DIRECTION ( 'NONE',  ( -0.000000000000000000, -0.000000000000000000, -1.000000000000000000 ) ) ;
#1997 = CIRCLE ( 'NONE', #4923, 3.000000000000002665 ) ;
#1998 = CARTESIAN_POINT ( 'NONE',  ( 35.00000000000000000, -5.000000000000000000, 4.258610482196280173E-15 ) ) ;
#1999 = CARTESIAN_POINT ( 'NONE',  ( -11.98978967046166666, -34.10919265018085866, 2.932969818539081786 ) ) ;
#2000 = CARTESIAN_POINT ( 'NONE',  ( 15.06716847275090387, 33.15945890355548897, 59.19951139074275659 ) ) ;
#2001 = CYLINDRICAL_SURFACE ( 'NONE', #17292, 17.00000000000000711 ) ;
#2002 = CARTESIAN_POINT ( 'NONE',  ( 36.06598984771572702, 7.000000000000000000, -48.42385786802028491 ) ) ;
#2003 = EDGE_LOOP ( 'NONE', ( #10767, #8699, #15633, #17642 ) ) ;
#2004 = VERTEX_POINT ( 'NONE', #12399 ) ;
#2005 = EDGE_CURVE ( 'NONE', #4617, #5340, #5421, .T. ) ;
#2006 = ORIENTED_EDGE ( 'NONE', *, *, #3561, .T. ) ;
#2007 = EDGE_LOOP ( 'NONE', ( #10156, #21285, #13146, #10033 ) ) ;
#2008 = CARTESIAN_POINT ( 'NONE',  ( -16.00000000000000000, 20.00000000000000000, -102.0000000000000142 ) ) ;
#2009 = CARTESIAN_POINT ( 'NONE',  ( -24.10368028608786162, 26.10969099697611995, -3.000000000000011546 ) ) ;
#2010 = CARTESIAN_POINT ( 'NONE',  ( 35.00000000000000000, 39.00000000000000711, 49.99999999999999289 ) ) ;
#2011 = CARTESIAN_POINT ( 'NONE',  ( 34.99999999999980815, 40.00000000000000000, 52.89999999999922409 ) ) ;
#2012 = CARTESIAN_POINT ( 'NONE',  ( 0.03962180513328213832, 39.99999108785333135, 48.76479353913838821 ) ) ;
#2013 = CIRCLE ( 'NONE', #5327, 19.11328065563151668 ) ;
#2014 = EDGE_CURVE ( 'NONE', #15016, #3715, #20184, .T. ) ;
#2015 = VERTEX_POINT ( 'NONE', #14566 ) ;
#2016 = CIRCLE ( 'NONE', #19183, 19.99999999999999289 ) ;
#2017 = CYLINDRICAL_SURFACE ( 'NONE', #10457, 19.11328065563152379 ) ;
#2018 = CARTESIAN_POINT ( 'NONE',  ( -9.519381208426278107, 40.00000000000000711, -53.51361895679583114 ) ) ;
#2019 = DIRECTION ( 'NONE',  ( 0.000000000000000000, 0.000000000000000000, 1.000000000000000000 ) ) ;
#2020 = DIRECTION ( 'NONE',  ( -0.000000000000000000, -0.000000000000000000, 1.000000000000000000 ) ) ;
#2021 = VECTOR ( 'NONE', #8797, 1000.000000000000000 ) ;
#2022 = CARTESIAN_POINT ( 'NONE',  ( -23.65408649739100966, -22.22891329980539155, -2.999999999999995559 ) ) ;
#2023 = DIRECTION ( 'NONE',  ( -1.000000000000000000, -1.208970125616063644E-17, 0.000000000000000000 ) ) ;
#2024 = CARTESIAN_POINT ( 'NONE',  ( -10.39230484541309174, -1.500000000000011768, 5.999999999999708677 ) ) ;
#2025 = EDGE_LOOP ( 'NONE', ( #5795, #20438, #16358, #11845 ) ) ;
#2026 = CONICAL_SURFACE ( 'NONE', #12259, 2.099999999999997868, 1.029744258676653867 ) ;
#2027 = ORIENTED_EDGE ( 'NONE', *, *, #12241, .F. ) ;
#2028 = EDGE_CURVE ( 'NONE', #17302, #16867, #2252, .T. ) ;
#2029 = VECTOR ( 'NONE', #19162, 1000.000000000000000 ) ;
#2030 = VERTEX_POINT ( 'NONE', #21576 ) ;
#2031 = VECTOR ( 'NONE', #22330, 1000.000000000000000 ) ;
#2032 = FACE_OUTER_BOUND ( 'NONE', #17813, .T. ) ;
#2033 = CARTESIAN_POINT ( 'NONE',  ( 34.99999999999999289, 0.000000000000000000, -54.99999999999705835 ) ) ;
#2034 = EDGE_CURVE ( 'NONE', #14303, #14783, #12839, .T. ) ;
#2035 = EDGE_CURVE ( 'NONE', #15147, #2703, #10661, .T. ) ;
#2036 = CARTESIAN_POINT ( 'NONE',  ( 35.00000000000001421, 5.000000000000000000, 1.540743955509788682E-30 ) ) ;
#2037 = DIRECTION ( 'NONE',  ( 0.000000000000000000, 0.000000000000000000, 1.000000000000000000 ) ) ;
#2038 = CARTESIAN_POINT ( 'NONE',  ( -28.95348479018558407, 14.76298474240494940, 3.000000000000023537 ) ) ;
#2039 = CARTESIAN_POINT ( 'NONE',  ( 3.330669073875469621E-13, -1.110223024625156540E-13, -2.999999999999971578 ) ) ;
#2040 = CIRCLE ( 'NONE', #11912, 49.99999999999998579 ) ;
#2041 = CARTESIAN_POINT ( 'NONE',  ( -9.870870746768591886, 37.43479630316498685, -54.49920060631094998 ) ) ;
#2042 = DIRECTION ( 'NONE',  ( 0.000000000000000000, -0.000000000000000000, -1.000000000000000000 ) ) ;
#2043 = AXIS2_PLACEMENT_3D ( 'NONE', #16183, #14231, #1784 ) ;
#2044 = ORIENTED_EDGE ( 'NONE', *, *, #10253, .T. ) ;
#2045 = CARTESIAN_POINT ( 'NONE',  ( -35.00000000000000000, 40.00000000000000000, 1.387778780781445676E-14 ) ) ;
#2046 = DIRECTION ( 'NONE',  ( 6.505213034913038160E-19, 3.903127820947822896E-18, 1.000000000000000000 ) ) ;
#2047 = EDGE_CURVE ( 'NONE', #10753, #19175, #253, .T. ) ;
#2048 = DIRECTION ( 'NONE',  ( -0.000000000000000000, 1.000000000000000000, -0.000000000000000000 ) ) ;
#2049 = DIRECTION ( 'NONE',  ( 0.000000000000000000, 0.000000000000000000, -1.000000000000000000 ) ) ;
#2050 = AXIS2_PLACEMENT_3D ( 'NONE', #678, #5942, #19926 ) ;
#2051 = ORIENTED_EDGE ( 'NONE', *, *, #6256, .T. ) ;
#2052 = LINE ( 'NONE', #19474, #7529 ) ;
#2053 = DIRECTION ( 'NONE',  ( 0.000000000000000000, 0.000000000000000000, -1.000000000000000000 ) ) ;
#2054 = TOROIDAL_SURFACE ( 'NONE', #5721, 34.90673715956759082, 8.750000000000000000 ) ;
#2055 = VECTOR ( 'NONE', #12216, 1000.000000000000000 ) ;
#2056 = EDGE_LOOP ( 'NONE', ( #9955, #14243, #15268, #21628 ) ) ;
#2057 = VECTOR ( 'NONE', #18363, 1000.000000000000000 ) ;
#2058 = AXIS2_PLACEMENT_3D ( 'NONE', #10921, #17579, #5539 ) ;
#2059 = ORIENTED_EDGE ( 'NONE', *, *, #6843, .T. ) ;
#2060 = CARTESIAN_POINT ( 'NONE',  ( 0.7921581640248794853, 24.99916066338866116, 6.999720221269573273 ) ) ;
#2061 = DIRECTION ( 'NONE',  ( 0.000000000000000000, 0.000000000000000000, 1.000000000000000000 ) ) ;
#2062 = CARTESIAN_POINT ( 'NONE',  ( 4.683984772515712893E-15, 5.025303850726727362, -17.00000000000000711 ) ) ;
#2063 = B_SPLINE_CURVE_WITH_KNOTS ( 'NONE', 3,
 ( #16023, #3899, #12464, #2173 ),
 .UNSPECIFIED., .F., .F.,
 ( 4, 4 ),
 ( 9.715086407478086874E-07, 0.001929643240672472169 ),
 .UNSPECIFIED. ) ;
#2064 = DIRECTION ( 'NONE',  ( 0.000000000000000000, 1.000000000000000000, 0.000000000000000000 ) ) ;
#2065 = ORIENTED_EDGE ( 'NONE', *, *, #19552, .T. ) ;
#2066 = DIRECTION ( 'NONE',  ( 1.000000000000000000, 0.000000000000000000, 0.000000000000000000 ) ) ;
#2067 = CARTESIAN_POINT ( 'NONE',  ( -6.816848327306503030, 40.00000000000000000, 52.46798795272709981 ) ) ;
#2068 = ORIENTED_EDGE ( 'NONE', *, *, #6955, .T. ) ;
#2069 = CARTESIAN_POINT ( 'NONE',  ( -47.83731665821558465, 10.00000000000000000, 38.93845529828710283 ) ) ;
#2070 = ADVANCED_FACE ( 'NONE', ( #4157, #11129 ), #5758, .T. ) ;
#2071 = DIRECTION ( 'NONE',  ( 0.000000000000000000, 0.000000000000000000, 1.000000000000000000 ) ) ;
#2072 = EDGE_CURVE ( 'NONE', #22642, #15602, #17239, .T. ) ;
#2073 = DIRECTION ( 'NONE',  ( -0.000000000000000000, 1.000000000000000000, -0.000000000000000000 ) ) ;
#2074 = ORIENTED_EDGE ( 'NONE', *, *, #1422, .T. ) ;
#2075 = CARTESIAN_POINT ( 'NONE',  ( 30.07487443287998374, -12.31876324338282380, -7.000000000000006217 ) ) ;
#2076 = CARTESIAN_POINT ( 'NONE',  ( 42.50000000000000000, 10.00000000000000000, 44.99999999999999289 ) ) ;
#2077 = CARTESIAN_POINT ( 'NONE',  ( -2.229105529478774717, 39.97007248092597820, -50.38830888536040931 ) ) ;
#2078 = AXIS2_PLACEMENT_3D ( 'NONE', #2075, #9069, #5619 ) ;
#2079 = VERTEX_POINT ( 'NONE', #21454 ) ;
#2080 = LINE ( 'NONE', #5746, #14555 ) ;
#2081 = EDGE_CURVE ( 'NONE', #10039, #14190, #11408, .T. ) ;
#2082 = DIRECTION ( 'NONE',  ( -1.000000000000000000, 9.802091999852181989E-15, 0.000000000000000000 ) ) ;
#2083 = LINE ( 'NONE', #2429, #18051 ) ;
#2084 = AXIS2_PLACEMENT_3D ( 'NONE', #14630, #21635, #4220 ) ;
#2085 = ORIENTED_EDGE ( 'NONE', *, *, #12937, .F. ) ;
#2086 = ORIENTED_EDGE ( 'NONE', *, *, #4485, .F. ) ;
#2087 = CIRCLE ( 'NONE', #17827, 31.50000000000000711 ) ;
#2088 = ORIENTED_EDGE ( 'NONE', *, *, #16733, .T. ) ;
#2089 = AXIS2_PLACEMENT_3D ( 'NONE', #13590, #15322, #16836 ) ;
#2090 = ORIENTED_EDGE ( 'NONE', *, *, #14922, .F. ) ;
#2091 = CARTESIAN_POINT ( 'NONE',  ( 13.00000000000024336, -2.516660498395250745, -105.0010000000000048 ) ) ;
#2092 = ADVANCED_FACE ( 'NONE', ( #1978 ), #8960, .F. ) ;
#2093 = CARTESIAN_POINT ( 'NONE',  ( -29.33203831401591444, -20.06142356895425038, 3.000000000000049738 ) ) ;
#2094 = DIRECTION ( 'NONE',  ( 0.000000000000000000, 1.000000000000000000, -0.000000000000000000 ) ) ;
#2095 = EDGE_LOOP ( 'NONE', ( #17339, #14563, #19602, #12820, #491, #11785, #13566, #22488, #22666 ) ) ;
#2096 = DIRECTION ( 'NONE',  ( -6.505213034913038160E-19, -3.903127820947822896E-18, -1.000000000000000000 ) ) ;
#2097 = FACE_OUTER_BOUND ( 'NONE', #3973, .T. ) ;
#2098 = ORIENTED_EDGE ( 'NONE', *, *, #15554, .T. ) ;
#2099 = CARTESIAN_POINT ( 'NONE',  ( -29.33526866242094755, 22.15900668633769044, -2.800654218530477912 ) ) ;
#2100 = CARTESIAN_POINT ( 'NONE',  ( 35.00000000000001421, -5.000000000000000000, 4.999999999999997335 ) ) ;
#2101 = CARTESIAN_POINT ( 'NONE',  ( 31.11359284679418735, 4.918774254215718678, -6.999999999999999112 ) ) ;
#2102 = ORIENTED_EDGE ( 'NONE', *, *, #14902, .T. ) ;
#2103 = FACE_OUTER_BOUND ( 'NONE', #18603, .T. ) ;
#2104 = ORIENTED_EDGE ( 'NONE', *, *, #1673, .F. ) ;
#2105 = LINE ( 'NONE', #14117, #16305 ) ;
#2106 = AXIS2_PLACEMENT_3D ( 'NONE', #7588, #2317, #7363 ) ;
#2107 = DIRECTION ( 'NONE',  ( 0.000000000000000000, 0.000000000000000000, -1.000000000000000000 ) ) ;
#2108 = PRESENTATION_STYLE_ASSIGNMENT (( #9745 ) ) ;
#2109 = DIRECTION ( 'NONE',  ( 6.505213034913038160E-19, 3.903127820947822896E-18, 1.000000000000000000 ) ) ;
#2110 = ORIENTED_EDGE ( 'NONE', *, *, #14828, .F. ) ;
#2111 = DIRECTION ( 'NONE',  ( 1.000000000000000000, 0.000000000000000000, 0.000000000000000000 ) ) ;
#2112 = CIRCLE ( 'NONE', #14887, 10.00000000000000178 ) ;
#2113 = AXIS2_PLACEMENT_3D ( 'NONE', #6299, #2756, #13257 ) ;
#2114 = CARTESIAN_POINT ( 'NONE',  ( 19.23106185100178323, 25.51013774189591388, 60.43438466297350686 ) ) ;
#2115 = CARTESIAN_POINT ( 'NONE',  ( -35.00000000000058265, 39.97500000000000142, -57.50000000000076028 ) ) ;
#2116 = AXIS2_PLACEMENT_3D ( 'NONE', #4212, #18990, #17023 ) ;
#2117 = CARTESIAN_POINT ( 'NONE',  ( 10.58465497538991507, 37.06540556996028357, -54.84139108225040360 ) ) ;
#2119 = ORIENTED_EDGE ( 'NONE', *, *, #11671, .T. ) ;
#2118 = EDGE_CURVE ( 'NONE', #11218, #2374, #12851, .T. ) ;
#2120 = VERTEX_POINT ( 'NONE', #371 ) ;
#2121 = VECTOR ( 'NONE', #1376, 1000.000000000000114 ) ;
#2122 = EDGE_LOOP ( 'NONE', ( #20601, #21676 ) ) ;
#2123 = ORIENTED_EDGE ( 'NONE', *, *, #4379, .T. ) ;
#2124 = DIRECTION ( 'NONE',  ( -0.1421319796954322312, 0.000000000000000000, 0.9898477157360405787 ) ) ;
#2125 = EDGE_CURVE ( 'NONE', #14214, #22156, #21717, .T. ) ;
#2126 = CIRCLE ( 'NONE', #14914, 2.500000000000002220 ) ;
#2127 = DIRECTION ( 'NONE',  ( 1.000000000000000000, 0.000000000000000000, 0.000000000000000000 ) ) ;
#2128 = EDGE_CURVE ( 'NONE', #3791, #5986, #11323, .T. ) ;
#2129 = AXIS2_PLACEMENT_3D ( 'NONE', #20168, #18557, #11570 ) ;
#2130 = DIRECTION ( 'NONE',  ( 0.000000000000000000, 0.000000000000000000, 1.000000000000000000 ) ) ;
#2131 = AXIS2_PLACEMENT_3D ( 'NONE', #10243, #4658, #1100 ) ;
#2132 = DIRECTION ( 'NONE',  ( -0.000000000000000000, 1.000000000000000000, -0.000000000000000000 ) ) ;
#2133 = DIRECTION ( 'NONE',  ( 1.000000000000000000, 0.000000000000000000, 0.000000000000000000 ) ) ;
#2134 = VECTOR ( 'NONE', #21153, 1000.000000000000000 ) ;
#2135 = ORIENTED_EDGE ( 'NONE', *, *, #17290, .T. ) ;
#2136 = CARTESIAN_POINT ( 'NONE',  ( 19.05255888325771352, 10.99999999999989875, 2.999999999999995559 ) ) ;
#2137 = CYLINDRICAL_SURFACE ( 'NONE', #9464, 8.999999999999998224 ) ;
#2138 = DIRECTION ( 'NONE',  ( -1.000000000000000000, 1.084202172485504434E-16, 0.000000000000000000 ) ) ;
#2139 = FILL_AREA_STYLE_COLOUR ( '', #15684 ) ;
#2140 = EDGE_CURVE ( 'NONE', #19773, #877, #2555, .T. ) ;
#2141 = DIRECTION ( 'NONE',  ( -0.000000000000000000, -1.000000000000000000, -0.000000000000000000 ) ) ;
#2142 = DIRECTION ( 'NONE',  ( 0.000000000000000000, 1.000000000000000000, 0.000000000000000000 ) ) ;
#2143 = CIRCLE ( 'NONE', #12004, 31.50000000000000711 ) ;
#2144 = VECTOR ( 'NONE', #11426, 1000.000000000000000 ) ;
#2145 = CARTESIAN_POINT ( 'NONE',  ( 14.93538271375446946, 34.13396246814556889, 3.000000000000023537 ) ) ;
#2146 = B_SPLINE_CURVE_WITH_KNOTS ( 'NONE', 3,
 ( #945, #20198, #18703, #14900 ),
 .UNSPECIFIED., .F., .F.,
 ( 4, 4 ),
 ( 0.001893031756885906478, 0.003808480026564050377 ),
 .UNSPECIFIED. ) ;
#2147 = FACE_OUTER_BOUND ( 'NONE', #10095, .T. ) ;
#2148 = EDGE_CURVE ( 'NONE', #3138, #18756, #4223, .T. ) ;
#2149 = VECTOR ( 'NONE', #10534, 1000.000000000000000 ) ;
#2150 = ORIENTED_EDGE ( 'NONE', *, *, #12686, .F. ) ;
#2151 = ORIENTED_EDGE ( 'NONE', *, *, #14754, .T. ) ;
#2152 = ORIENTED_EDGE ( 'NONE', *, *, #13561, .T. ) ;
#2153 = ADVANCED_FACE ( 'NONE', ( #9642, #16632 ), #22255, .F. ) ;
#2154 = CYLINDRICAL_SURFACE ( 'NONE', #13661, 31.50000000000000711 ) ;
#2155 = AXIS2_PLACEMENT_3D ( 'NONE', #4219, #14847, #12678 ) ;
#2156 = CARTESIAN_POINT ( 'NONE',  ( -35.00000000000000000, 0.000000000000000000, -40.99999999999997868 ) ) ;
#2157 = CARTESIAN_POINT ( 'NONE',  ( 0.000000000000000000, 10.00000000000000000, 0.000000000000000000 ) ) ;
#2158 = DIRECTION ( 'NONE',  ( -0.000000000000000000, 1.000000000000000000, -0.000000000000000000 ) ) ;
#2159 = DIRECTION ( 'NONE',  ( -0.000000000000000000, -1.000000000000000000, -0.000000000000000000 ) ) ;
#2160 = CARTESIAN_POINT ( 'NONE',  ( -10.00000000000000000, 1.499999999999997780, 3.000000000000000000 ) ) ;
#2161 = CARTESIAN_POINT ( 'NONE',  ( -15.89815672374914080, 32.14246426897781816, -59.47617874060593124 ) ) ;
#2162 = CARTESIAN_POINT ( 'NONE',  ( 5.551115123125782702E-14, -1.387778780781445676E-13, -5.749999999999949374 ) ) ;
#2163 = EDGE_CURVE ( 'NONE', #17952, #22537, #11802, .T. ) ;
#2164 = ORIENTED_EDGE ( 'NONE', *, *, #16598, .T. ) ;
#2165 = LINE ( 'NONE', #17398, #16809 ) ;
#2166 = DIRECTION ( 'NONE',  ( 6.505213034913038160E-19, 3.903127820947822896E-18, 1.000000000000000000 ) ) ;
#2167 = CARTESIAN_POINT ( 'NONE',  ( 10.63866000424712688, 9.419394561690120682, -43.66469350997162024 ) ) ;
#2168 = VERTEX_POINT ( 'NONE', #13514 ) ;
#2169 = COLOUR_RGB ( '',0.7921568627450980005, 0.8196078431372548767, 0.9333333333333333481 ) ;
#2170 = DIRECTION ( 'NONE',  ( 6.505213034913038160E-19, 3.903127820947822896E-18, 1.000000000000000000 ) ) ;
#2171 = CARTESIAN_POINT ( 'NONE',  ( 5.999999999999999112, -40.00000000000000000, -6.000000000000000000 ) ) ;
#2172 = ADVANCED_FACE ( 'NONE', ( #9969 ), #17298, .T. ) ;
#2173 = CARTESIAN_POINT ( 'NONE',  ( -19.59430950039299546, 28.88846368933323205, 2.999999999999995559 ) ) ;
#2174 = EDGE_LOOP ( 'NONE', ( #6678, #9947, #19944, #8878 ) ) ;
#2175 = ADVANCED_FACE ( 'NONE', ( #8716 ), #1271, .F. ) ;
#2176 = EDGE_LOOP ( 'NONE', ( #8644, #3320, #15371, #20064, #8776, #7471 ) ) ;
#2177 = CARTESIAN_POINT ( 'NONE',  ( -4.153516728483839238, 35.28654656445758064, 3.000000000000046629 ) ) ;
#2178 = CARTESIAN_POINT ( 'NONE',  ( -13.56354382738803466, 2.142135623730931471, 56.03997097393687454 ) ) ;
#2179 = B_SPLINE_CURVE_WITH_KNOTS ( 'NONE', 3,
 ( #22425, #11757, #13685, #3297, #8215, #20700, #6607, #13571, #998, #1115, #11537, #1335, #11868, #18526, #11991, #20253, #18991 ),
 .UNSPECIFIED., .F., .F.,
 ( 4, 1, 1, 2, 2, 1, 1, 1, 2, 2, 4 ),
 ( 0.000000000000000000, 0.1250000000000117129, 0.1875000000000175693, 0.2187500000000204836, 0.2500000000000234257, 0.3750000000000403566, 0.4375000000000473510, 0.4687500000000494049, 0.4843750000000508482, 0.5000000000000522915, 1.000000000000000000 ),
 .UNSPECIFIED. ) ;
#2180 = DIRECTION ( 'NONE',  ( -0.000000000000000000, -0.000000000000000000, 1.000000000000000000 ) ) ;
#2181 = ORIENTED_EDGE ( 'NONE', *, *, #8709, .T. ) ;
#2182 = FACE_OUTER_BOUND ( 'NONE', #17675, .T. ) ;
#2183 = CARTESIAN_POINT ( 'NONE',  ( -5.553309044144580042, 39.99999999999999289, 51.88330199943927568 ) ) ;
#2184 = ORIENTED_EDGE ( 'NONE', *, *, #15752, .F. ) ;
#2185 = CARTESIAN_POINT ( 'NONE',  ( 29.33526866242106124, -22.15900668633785742, 2.800654218530492123 ) ) ;
#2186 = DIRECTION ( 'NONE',  ( 0.000000000000000000, -1.000000000000000000, 0.000000000000000000 ) ) ;
#2187 = DIRECTION ( 'NONE',  ( -1.000000000000000000, -9.076011110974242363E-16, 0.000000000000000000 ) ) ;
#2188 = LINE ( 'NONE', #12713, #13951 ) ;
#2189 = ADVANCED_FACE ( 'NONE', ( #6551 ), #19147, .T. ) ;
#2190 = VERTEX_POINT ( 'NONE', #16963 ) ;
#2191 = DIRECTION ( 'NONE',  ( -0.000000000000000000, -0.000000000000000000, 1.000000000000000000 ) ) ;
#2192 = FACE_OUTER_BOUND ( 'NONE', #12078, .T. ) ;
#2193 = CARTESIAN_POINT ( 'NONE',  ( -6.692425220448997791, 39.70962082156066231, -53.18141015372126645 ) ) ;
#2194 = ORIENTED_EDGE ( 'NONE', *, *, #14920, .F. ) ;
#2195 = CONICAL_SURFACE ( 'NONE', #21971, 15.00000000000000000, 0.7853981633974552734 ) ;
#2196 = DIRECTION ( 'NONE',  ( -0.000000000000000000, 1.000000000000000000, -0.000000000000000000 ) ) ;
#2197 = CARTESIAN_POINT ( 'NONE',  ( 35.00000000000058265, 26.00000000000000355, -52.90000000000076597 ) ) ;
#2198 = CIRCLE ( 'NONE', #18295, 25.00000000000000711 ) ;
#2200 = EDGE_CURVE ( 'NONE', #20280, #8421, #7747, .T. ) ;
#2199 = VERTEX_POINT ( 'NONE', #15694 ) ;
#2201 = EDGE_CURVE ( 'NONE', #11720, #12153, #8, .T. ) ;
#2202 = VERTEX_POINT ( 'NONE', #1614 ) ;
#2203 = ORIENTED_EDGE ( 'NONE', *, *, #13624, .F. ) ;
#2204 =( NAMED_UNIT ( * ) PLANE_ANGLE_UNIT ( ) SI_UNIT ( $, .RADIAN. ) );
#2205 = ORIENTED_EDGE ( 'NONE', *, *, #15691, .F. ) ;
#2206 = CYLINDRICAL_SURFACE ( 'NONE', #56, 2.499999999999998668 ) ;
#2207 = CYLINDRICAL_SURFACE ( 'NONE', #18576, 1.000000000000000888 ) ;
#2208 = TOROIDAL_SURFACE ( 'NONE', #18687, 18.00000000000000711, 0.9999999999999985567 ) ;
#2209 = CARTESIAN_POINT ( 'NONE',  ( 9.225361348764007374, 39.40776743449596609, -54.37884520109041375 ) ) ;
#2210 = CARTESIAN_POINT ( 'NONE',  ( -3.000000000000000000, 16.00000000000000000, 8.485281374238567764 ) ) ;
#2211 = EDGE_CURVE ( 'NONE', #9264, #10753, #8115, .T. ) ;
#2212 = EDGE_LOOP ( 'NONE', ( #18111, #16152 ) ) ;
#2213 = DIRECTION ( 'NONE',  ( -6.505213034913038160E-19, -3.903127820947822896E-18, -1.000000000000000000 ) ) ;
#2214 = FACE_OUTER_BOUND ( 'NONE', #13033, .T. ) ;
#2215 = ORIENTED_EDGE ( 'NONE', *, *, #3324, .T. ) ;
#2216 = CARTESIAN_POINT ( 'NONE',  ( 35.00000000000058265, 40.00000000000000711, -55.00000000000076028 ) ) ;
#2217 = CARTESIAN_POINT ( 'NONE',  ( -11.86180952233172725, 39.00000000000000000, -55.35904751184885697 ) ) ;
#2218 = DIRECTION ( 'NONE',  ( -0.000000000000000000, -1.000000000000000000, -0.000000000000000000 ) ) ;
#2219 = ORIENTED_EDGE ( 'NONE', *, *, #19831, .T. ) ;
#2220 = DIRECTION ( 'NONE',  ( -0.000000000000000000, 1.000000000000000000, -0.000000000000000000 ) ) ;
#2221 = VERTEX_POINT ( 'NONE', #3002 ) ;
#2222 = CARTESIAN_POINT ( 'NONE',  ( -4.171001175319544174, -35.79662727779886211, -2.999999999999995559 ) ) ;
#2223 = CARTESIAN_POINT ( 'NONE',  ( 6.696867368502865039E-15, 35.00000000000000000, 38.73397172404480671 ) ) ;
#2224 = CARTESIAN_POINT ( 'NONE',  ( -42.50000000000000711, -11.97499999999999964, 50.00000000000000711 ) ) ;
#2225 = EDGE_LOOP ( 'NONE', ( #19995, #18967 ) ) ;
#2226 = CARTESIAN_POINT ( 'NONE',  ( -11.85401191286875111, -32.83234229683740324, 3.000000000000023537 ) ) ;
#2227 = CARTESIAN_POINT ( 'NONE',  ( 20.31722544680816256, 29.72987180553230502, 58.17992760854182421 ) ) ;
#2228 = CARTESIAN_POINT ( 'NONE',  ( 26.10969099697632956, 24.10368028608786517, -3.000000000000007105 ) ) ;
#2229 = AXIS2_PLACEMENT_3D ( 'NONE', #3378, #1426, #5315 ) ;
#2230 = CARTESIAN_POINT ( 'NONE',  ( -35.00000000000000000, 39.00000000000000711, 1.387778780781445676E-14 ) ) ;
#2232 = EDGE_CURVE ( 'NONE', #19255, #15800, #10651, .T. ) ;
#2231 = ORIENTED_EDGE ( 'NONE', *, *, #5568, .F. ) ;
#2233 = ORIENTED_EDGE ( 'NONE', *, *, #17462, .T. ) ;
#2234 = ORIENTED_EDGE ( 'NONE', *, *, #20437, .T. ) ;
#2235 = ORIENTED_EDGE ( 'NONE', *, *, #4469, .F. ) ;
#2236 = DIRECTION ( 'NONE',  ( 0.000000000000000000, 0.000000000000000000, -1.000000000000000000 ) ) ;
#2237 = CARTESIAN_POINT ( 'NONE',  ( -35.00000000000000000, 13.99999999999999822, 2.255140518769849223E-14 ) ) ;
#2238 = LINE ( 'NONE', #2010, #14014 ) ;
#2239 = EDGE_CURVE ( 'NONE', #5417, #22152, #1154, .T. ) ;
#2240 = ORIENTED_EDGE ( 'NONE', *, *, #12614, .F. ) ;
#2241 = CARTESIAN_POINT ( 'NONE',  ( -13.83143812983110621, 29.36548507648009831, -2.999999999999995559 ) ) ;
#2242 = CARTESIAN_POINT ( 'NONE',  ( 42.49999999999998579, 10.00000000000000000, -53.99999999999997868 ) ) ;
#2243 = VERTEX_POINT ( 'NONE', #19038 ) ;
#2244 = CARTESIAN_POINT ( 'NONE',  ( -28.96193690644918561, -14.74639653023249153, -2.999999999999988898 ) ) ;
#2245 = PRODUCT_DEFINITION_CONTEXT ( 'detailed design', #5637, 'design' ) ;
#2246 = CARTESIAN_POINT ( 'NONE',  ( 28.45046755804905914, -15.62726112422602220, -7.000000000000006217 ) ) ;
#2247 = CARTESIAN_POINT ( 'NONE',  ( -42.49999999999996447, 10.00000000000000000, -47.50000000000000711 ) ) ;
#2248 = CARTESIAN_POINT ( 'NONE',  ( 25.00000000000000000, 20.00000000000000000, 6.487780019669002523E-15 ) ) ;
#2249 = EDGE_CURVE ( 'NONE', #21816, #7482, #4094, .T. ) ;
#2250 = DIRECTION ( 'NONE',  ( 0.000000000000000000, 0.000000000000000000, 1.000000000000000000 ) ) ;
#2251 = ADVANCED_FACE ( 'NONE', ( #20753 ), #9578, .F. ) ;
#2252 = CIRCLE ( 'NONE', #19087, 28.00000000000001066 ) ;
#2253 = AXIS2_PLACEMENT_3D ( 'NONE', #8380, #11803, #11922 ) ;
#2254 = CARTESIAN_POINT ( 'NONE',  ( -18.83615802559791774, 32.14641817400182333, 2.999999999999995559 ) ) ;
#2255 = CARTESIAN_POINT ( 'NONE',  ( 35.00000000000000000, -9.000000000000001776, 18.00000000000000711 ) ) ;
#2256 = ORIENTED_EDGE ( 'NONE', *, *, #13298, .F. ) ;
#2257 = EDGE_LOOP ( 'NONE', ( #1570, #15899 ) ) ;
#2258 = ORIENTED_EDGE ( 'NONE', *, *, #2366, .F. ) ;
#2259 = CARTESIAN_POINT ( 'NONE',  ( -5.999999999999998224, -20.00000000000000000, 5.999999999999999112 ) ) ;
#2260 = CARTESIAN_POINT ( 'NONE',  ( -6.262904276180248253, 0.9586397763588609955, -54.84547588849994781 ) ) ;
#2261 = DIRECTION ( 'NONE',  ( 0.000000000000000000, 1.000000000000000000, 0.000000000000000000 ) ) ;
#2262 = VECTOR ( 'NONE', #14767, 1000.000000000000000 ) ;
#2263 = DIRECTION ( 'NONE',  ( 1.000000000000000000, 1.208970125616053321E-17, 0.000000000000000000 ) ) ;
#2264 = DIRECTION ( 'NONE',  ( 1.296372316667914327E-16, 1.000000000000000000, -0.000000000000000000 ) ) ;
#2265 = CARTESIAN_POINT ( 'NONE',  ( -19.80871821058217108, 17.21148610482000763, 60.57629886234796857 ) ) ;
#2266 = EDGE_CURVE ( 'NONE', #8449, #4746, #10218, .T. ) ;
#2267 = CARTESIAN_POINT ( 'NONE',  ( -12.26943921815750116, 35.80002840870906766, -58.15275698935778337 ) ) ;
#2268 = DIRECTION ( 'NONE',  ( 0.000000000000000000, -1.000000000000000000, 0.000000000000000000 ) ) ;
#2269 = ORIENTED_EDGE ( 'NONE', *, *, #22339, .F. ) ;
#2270 = CARTESIAN_POINT ( 'NONE',  ( 1.110223024625156540E-13, -5.551115123125782702E-14, -6.999999999999950262 ) ) ;
#2271 = CARTESIAN_POINT ( 'NONE',  ( 42.50000000000000000, 7.000000000000000000, 47.49999999999999289 ) ) ;
#2272 = DIRECTION ( 'NONE',  ( 0.000000000000000000, 0.000000000000000000, 1.000000000000000000 ) ) ;
#2273 = LINE ( 'NONE', #16242, #18852 ) ;
#2274 = FACE_OUTER_BOUND ( 'NONE', #4306, .T. ) ;
#2275 = ORIENTED_EDGE ( 'NONE', *, *, #13053, .T. ) ;
#2276 = CARTESIAN_POINT ( 'NONE',  ( -19.99999999999979394, -2.775557561562891351E-14, -2.999999999999971578 ) ) ;
#2277 = VERTEX_POINT ( 'NONE', #11920 ) ;
#2278 = DIRECTION ( 'NONE',  ( 6.505213034913038160E-19, 3.903127820947822896E-18, 1.000000000000000000 ) ) ;
#2279 = CARTESIAN_POINT ( 'NONE',  ( 13.00000000000000178, 20.00000000000000000, -11.32475165290605901 ) ) ;
#2280 = FACE_BOUND ( 'NONE', #20023, .T. ) ;
#2281 = AXIS2_PLACEMENT_3D ( 'NONE', #20000, #13098, #16664 ) ;
#2282 = ORIENTED_EDGE ( 'NONE', *, *, #17720, .F. ) ;
#2283 = CARTESIAN_POINT ( 'NONE',  ( -30.13956425491233659, -21.05198877411806890, -2.000000000000001776 ) ) ;
#2284 = ADVANCED_FACE ( 'NONE', ( #18920 ), #10196, .F. ) ;
#2285 = ORIENTED_EDGE ( 'NONE', *, *, #3044, .T. ) ;
#2286 = CARTESIAN_POINT ( 'NONE',  ( -4.025500340002485800, 36.54278193890309012, 2.800654218530485018 ) ) ;
#2287 = FACE_OUTER_BOUND ( 'NONE', #20245, .T. ) ;
#2288 = CYLINDRICAL_SURFACE ( 'NONE', #7270, 0.9999999999999974465 ) ;
#2289 = ORIENTED_EDGE ( 'NONE', *, *, #14020, .T. ) ;
#2290 = CARTESIAN_POINT ( 'NONE',  ( -12.84899528830096926, 2.142135623730930583, 57.90797000640143466 ) ) ;
#2291 = CARTESIAN_POINT ( 'NONE',  ( -27.19760187735847978, -24.73600648735121865, -1.999999999999977573 ) ) ;
#2292 = VERTEX_POINT ( 'NONE', #15574 ) ;
#2293 = CARTESIAN_POINT ( 'NONE',  ( -17.99999999999980460, -8.348434146949763185E-14, 4.999999999999993783 ) ) ;
#2294 = EDGE_CURVE ( 'NONE', #2966, #18701, #22597, .T. ) ;
#2296 = EDGE_CURVE ( 'NONE', #10675, #16483, #414, .T. ) ;
#2295 = DIRECTION ( 'NONE',  ( 1.000000000000000000, 0.000000000000000000, 0.000000000000000000 ) ) ;
#2297 = CARTESIAN_POINT ( 'NONE',  ( 25.99999999999998579, 19.99999999999999645, -100.0000000000000000 ) ) ;
#2298 = CARTESIAN_POINT ( 'NONE',  ( 35.99819890246955367, -7.463862311151231665, -2.000000000000001776 ) ) ;
#2299 = ORIENTED_EDGE ( 'NONE', *, *, #11532, .F. ) ;
#2300 = LINE ( 'NONE', #12827, #21107 ) ;
#2301 = CARTESIAN_POINT ( 'NONE',  ( -13.56354382738793696, 2.142135623730796468, 56.03997097393716587 ) ) ;
#2302 = CARTESIAN_POINT ( 'NONE',  ( -3.069014598162472129, 39.94370170965071765, -50.97148269059585601 ) ) ;
#2303 = AXIS2_PLACEMENT_3D ( 'NONE', #22413, #10246, #8983 ) ;
#2304 = VERTEX_POINT ( 'NONE', #569 ) ;
#2305 = CARTESIAN_POINT ( 'NONE',  ( 10.62139969368200454, 0.6004703193300734432, 54.70636795414621645 ) ) ;
#2306 = DIRECTION ( 'NONE',  ( -1.000000000000000000, 0.000000000000000000, 1.445602896647339410E-16 ) ) ;
#2307 = DIRECTION ( 'NONE',  ( 1.296372316667914327E-16, 1.000000000000000000, -0.000000000000000000 ) ) ;
#2308 = VERTEX_POINT ( 'NONE', #5284 ) ;
#2309 = VECTOR ( 'NONE', #22199, 1000.000000000000000 ) ;
#2310 = EDGE_LOOP ( 'NONE', ( #20692, #6820, #17268, #1015, #21602, #6129 ) ) ;
#2311 = ADVANCED_FACE ( 'NONE', ( #15795 ), #22083, .T. ) ;
#2312 = ORIENTED_EDGE ( 'NONE', *, *, #5126, .F. ) ;
#2313 = CIRCLE ( 'NONE', #15101, 18.00000000000000000 ) ;
#2314 = CIRCLE ( 'NONE', #18793, 39.00000000000001421 ) ;
#2315 = ORIENTED_EDGE ( 'NONE', *, *, #18484, .T. ) ;
#2316 = FACE_OUTER_BOUND ( 'NONE', #2660, .T. ) ;
#2317 = DIRECTION ( 'NONE',  ( 0.000000000000000000, -1.000000000000000000, 0.000000000000000000 ) ) ;
#2318 = DIRECTION ( 'NONE',  ( -6.505213034913038160E-19, -3.903127820947822896E-18, -1.000000000000000000 ) ) ;
#2319 = LINE ( 'NONE', #4389, #6 ) ;
#2320 = ORIENTED_EDGE ( 'NONE', *, *, #16902, .T. ) ;
#2321 = CARTESIAN_POINT ( 'NONE',  ( -18.83615802559775076, 32.14641817400176649, -2.999999999999971578 ) ) ;
#2322 = CARTESIAN_POINT ( 'NONE',  ( -30.48934413892756368, 16.99647590252650886, -2.999999999999995559 ) ) ;
#2323 = ORIENTED_EDGE ( 'NONE', *, *, #21288, .T. ) ;
#2324 = EDGE_CURVE ( 'NONE', #17065, #6302, #3364, .T. ) ;
#2325 = ADVANCED_FACE ( 'NONE', ( #17981 ), #7102, .F. ) ;
#2326 = DIRECTION ( 'NONE',  ( -1.000000000000000000, -1.208970125616077665E-17, 0.000000000000000000 ) ) ;
#2327 = CARTESIAN_POINT ( 'NONE',  ( -33.51030287062352642, -15.12081897056683033, 2.800654218530502337 ) ) ;
#2328 = CARTESIAN_POINT ( 'NONE',  ( -21.65063509461097269, 12.49999999999990052, -5.000000000000004441 ) ) ;
#2329 = ORIENTED_EDGE ( 'NONE', *, *, #1957, .T. ) ;
#2330 = CIRCLE ( 'NONE', #15851, 19.11328065563152023 ) ;
#2331 = DIRECTION ( 'NONE',  ( -0.000000000000000000, -1.000000000000000000, -0.000000000000000000 ) ) ;
#2332 = VERTEX_POINT ( 'NONE', #12582 ) ;
#2333 = DIRECTION ( 'NONE',  ( -0.000000000000000000, 1.000000000000000000, -0.000000000000000000 ) ) ;
#2334 = CARTESIAN_POINT ( 'NONE',  ( -35.00000000000000000, -15.00000000000000000, 2.255140518769849223E-14 ) ) ;
#2335 = EDGE_CURVE ( 'NONE', #1842, #1434, #12463, .T. ) ;
#2336 = CARTESIAN_POINT ( 'NONE',  ( 3.126261098509322434, 0.2355326842376759267, 52.75562998449589003 ) ) ;
#2337 = ORIENTED_EDGE ( 'NONE', *, *, #18707, .F. ) ;
#2338 = DIRECTION ( 'NONE',  ( -0.000000000000000000, 1.000000000000000000, -0.000000000000000000 ) ) ;
#2339 = AXIS2_PLACEMENT_3D ( 'NONE', #13019, #1008, #21638 ) ;
#2340 = CARTESIAN_POINT ( 'NONE',  ( 12.50843255120944875, 35.62740313860285113, 55.64392373821144133 ) ) ;
#2341 = ADVANCED_FACE ( 'NONE', ( #16259 ), #19718, .T. ) ;
#2342 = DIRECTION ( 'NONE',  ( 1.000000000000000000, 0.000000000000000000, 0.000000000000000000 ) ) ;
#2343 = VECTOR ( 'NONE', #13022, 1000.000000000000000 ) ;
#2344 = VECTOR ( 'NONE', #3447, 1000.000000000000000 ) ;
#2345 = DIRECTION ( 'NONE',  ( -6.505213034913038160E-19, -3.903127820947822896E-18, -1.000000000000000000 ) ) ;
#2346 = EDGE_LOOP ( 'NONE', ( #12465, #20087, #1961, #7729 ) ) ;
#2347 = AXIS2_PLACEMENT_3D ( 'NONE', #7152, #8652, #21143 ) ;
#2348 = ORIENTED_EDGE ( 'NONE', *, *, #5691, .F. ) ;
#2349 = ORIENTED_EDGE ( 'NONE', *, *, #14496, .T. ) ;
#2350 = VERTEX_POINT ( 'NONE', #7215 ) ;
#2351 = CARTESIAN_POINT ( 'NONE',  ( 41.39271818392635538, 10.00000000000000000, 5.943569790512533757 ) ) ;
#2352 = DIRECTION ( 'NONE',  ( 0.000000000000000000, 0.000000000000000000, 1.000000000000000000 ) ) ;
#2353 = CIRCLE ( 'NONE', #5280, 2.500000000000002220 ) ;
#2354 = DIRECTION ( 'NONE',  ( -6.505213034913038160E-19, -3.903127820947822896E-18, -1.000000000000000000 ) ) ;
#2355 = ORIENTED_EDGE ( 'NONE', *, *, #4969, .F. ) ;
#2356 = DIRECTION ( 'NONE',  ( 6.505213034913038160E-19, 3.903127820947822896E-18, 1.000000000000000000 ) ) ;
#2357 = DIRECTION ( 'NONE',  ( 0.000000000000000000, 0.000000000000000000, 1.000000000000000000 ) ) ;
#2358 = AXIS2_PLACEMENT_3D ( 'NONE', #94, #10399, #19249 ) ;
#2360 = ORIENTED_EDGE ( 'NONE', *, *, #12885, .T. ) ;
#2359 = B_SPLINE_CURVE_WITH_KNOTS ( 'NONE', 3,
 ( #20809, #5120, #6828, #13792 ),
 .UNSPECIFIED., .F., .F.,
 ( 4, 4 ),
 ( 9.715086431275246711E-07, 0.001929643240674561860 ),
 .UNSPECIFIED. ) ;
#2361 = CARTESIAN_POINT ( 'NONE',  ( -42.50000000000000711, -12.00000000000012434, -44.97499999999988773 ) ) ;
#2362 = DIRECTION ( 'NONE',  ( -1.000000000000000000, 1.371829164384562918E-16, 0.000000000000000000 ) ) ;
#2363 = DIRECTION ( 'NONE',  ( 0.000000000000000000, 0.000000000000000000, -1.000000000000000000 ) ) ;
#2364 = CARTESIAN_POINT ( 'NONE',  ( -11.68090480754633731, 3.765577839755393619, -57.90797000640141334 ) ) ;
#2365 = EDGE_CURVE ( 'NONE', #18225, #21604, #22661, .T. ) ;
#2366 = EDGE_CURVE ( 'NONE', #19351, #478, #11387, .T. ) ;
#2367 = VECTOR ( 'NONE', #10808, 1000.000000000000000 ) ;
#2368 = DIRECTION ( 'NONE',  ( 0.000000000000000000, 0.000000000000000000, 1.000000000000000000 ) ) ;
#2369 = AXIS2_PLACEMENT_3D ( 'NONE', #22218, #1469, #20718 ) ;
#2370 = DIRECTION ( 'NONE',  ( 1.000000000000000000, 1.208970125616062874E-17, 0.000000000000000000 ) ) ;
#2371 = EDGE_CURVE ( 'NONE', #4794, #18735, #1566, .T. ) ;
#2372 = CARTESIAN_POINT ( 'NONE',  ( 21.99999999999998579, 20.00000000000000000, 100.0000000000000000 ) ) ;
#2373 = ORIENTED_EDGE ( 'NONE', *, *, #16600, .T. ) ;
#2374 = VERTEX_POINT ( 'NONE', #16605 ) ;
#2375 = VERTEX_POINT ( 'NONE', #8023 ) ;
#2376 = CARTESIAN_POINT ( 'NONE',  ( 9.000000000000005329, 12.49999999999999467, 0.000000000000000000 ) ) ;
#2377 = CLOSED_SHELL ( 'NONE', ( #15840, #2588, #18828, #3195, #14125, #19318, #13827, #6682, #21945, #10747, #17338, #14273, #22672, #14010, #8312, #12983, #9918, #6676, #7246, #21227, #12866, #3900, #16028, #2189, #18705, #11982, #13364, #12111, #21806, #17586, #11435, #17237, #8288, #21448, #10491, #16012, #20701, #9854 ) ) ;
#2378 = LINE ( 'NONE', #18404, #11244 ) ;
#2379 = VECTOR ( 'NONE', #15019, 1000.000000000000114 ) ;
#2380 = EDGE_CURVE ( 'NONE', #8634, #18457, #2887, .T. ) ;
#2381 = CARTESIAN_POINT ( 'NONE',  ( 90.00000000000000000, 28.00000000000000000, 2.099999999999989875 ) ) ;
#2382 = LINE ( 'NONE', #13688, #15205 ) ;
#2383 = CARTESIAN_POINT ( 'NONE',  ( -1.387778780781445518E-14, 20.00000000000000355, 105.0000000000000142 ) ) ;
#2384 = CARTESIAN_POINT ( 'NONE',  ( -1.427806064787912943, 39.96253293977173371, -50.08434658998346123 ) ) ;
#2385 = DIRECTION ( 'NONE',  ( 0.000000000000000000, 1.000000000000000000, 0.000000000000000000 ) ) ;
#2386 = DIRECTION ( 'NONE',  ( 0.000000000000000000, 1.000000000000000000, -0.000000000000000000 ) ) ;
#2387 = DIRECTION ( 'NONE',  ( 6.505213034913038160E-19, 3.903127820947822896E-18, 1.000000000000000000 ) ) ;
#2388 = VERTEX_POINT ( 'NONE', #10481 ) ;
#2389 = CARTESIAN_POINT ( 'NONE',  ( 37.07861450834834471, -3.656418565264496490, -2.999999999999971578 ) ) ;
#2390 = CARTESIAN_POINT ( 'NONE',  ( 42.50000000000000711, -12.00000000000000000, 54.00000000000000711 ) ) ;
#2391 = DIRECTION ( 'NONE',  ( 0.000000000000000000, 0.000000000000000000, 1.000000000000000000 ) ) ;
#2392 = CARTESIAN_POINT ( 'NONE',  ( -34.99999999999999289, -3.999999999999985345, -3.012171160963566127E-14 ) ) ;
#2393 = CONICAL_SURFACE ( 'NONE', #10411, 59.99999999999700862, 0.7853981633974380649 ) ;
#2394 = ORIENTED_EDGE ( 'NONE', *, *, #1237, .T. ) ;
#2395 = DIRECTION ( 'NONE',  ( -6.505213034913038160E-19, -3.903127820947822896E-18, -1.000000000000000000 ) ) ;
#2396 = AXIS2_PLACEMENT_3D ( 'NONE', #17885, #21211, #7342 ) ;
#2397 = CARTESIAN_POINT ( 'NONE',  ( 17.99999999999998579, 20.00000000000000711, -102.9999999999999716 ) ) ;
#2398 = DIRECTION ( 'NONE',  ( -0.000000000000000000, -1.000000000000000000, -0.000000000000000000 ) ) ;
#2399 = DIRECTION ( 'NONE',  ( -1.000000000000000000, 0.000000000000000000, 0.000000000000000000 ) ) ;
#2400 = VECTOR ( 'NONE', #18818, 1000.000000000000000 ) ;
#2401 = ORIENTED_EDGE ( 'NONE', *, *, #2034, .T. ) ;
#2402 = EDGE_CURVE ( 'NONE', #12588, #11670, #15669, .T. ) ;
#2403 = DIRECTION ( 'NONE',  ( 0.000000000000000000, 0.5150380749100562650, 0.8571673007021111124 ) ) ;
#2404 = PRODUCT_RELATED_PRODUCT_CATEGORY ( 'part', '', ( #12944 ) ) ;
#2405 = CARTESIAN_POINT ( 'NONE',  ( 3.092931222847586259, 39.99999999999999289, -50.60141000603072570 ) ) ;
#2406 = AXIS2_PLACEMENT_3D ( 'NONE', #14824, #16334, #9687 ) ;
#2407 = VERTEX_POINT ( 'NONE', #12428 ) ;
#2408 = CARTESIAN_POINT ( 'NONE',  ( 0.3010984638803619884, 39.99946791130895463, -48.96692764038679258 ) ) ;
#2409 = AXIS2_PLACEMENT_3D ( 'NONE', #5465, #12657, #10951 ) ;
#2410 = CARTESIAN_POINT ( 'NONE',  ( 11.87329829275380533, 39.99999999999997868, 54.28004929202755591 ) ) ;
#2411 = DIRECTION ( 'NONE',  ( 0.000000000000000000, 1.000000000000000000, 0.000000000000000000 ) ) ;
#2412 = ORIENTED_EDGE ( 'NONE', *, *, #13612, .F. ) ;
#2413 = CARTESIAN_POINT ( 'NONE',  ( -90.00000000000000000, 40.00000000000000711, 2.524999999999998579 ) ) ;
#2414 = CARTESIAN_POINT ( 'NONE',  ( -11.05758567242951607, 3.294696707132223512, -55.18338768060504407 ) ) ;
#2415 = ORIENTED_EDGE ( 'NONE', *, *, #1505, .T. ) ;
#2416 = AXIS2_PLACEMENT_3D ( 'NONE', #1603, #15788, #10406 ) ;
#2417 = DIRECTION ( 'NONE',  ( 0.000000000000000000, 0.000000000000000000, 1.000000000000000000 ) ) ;
#2418 = CARTESIAN_POINT ( 'NONE',  ( -5.649790292151565474, 40.00000000000000711, 51.93142534747384786 ) ) ;
#2419 = AXIS2_PLACEMENT_3D ( 'NONE', #20940, #1689, #8221 ) ;
#2420 = CARTESIAN_POINT ( 'NONE',  ( 3.608224830031758756E-13, -2.775557561562891351E-14, -4.999999999999997335 ) ) ;
#2421 = VERTEX_POINT ( 'NONE', #8784 ) ;
#2422 = FACE_OUTER_BOUND ( 'NONE', #8100, .T. ) ;
#2423 = DIRECTION ( 'NONE',  ( -0.000000000000000000, 1.000000000000000000, -0.000000000000000000 ) ) ;
#2424 = CARTESIAN_POINT ( 'NONE',  ( 12.00000000000000355, 1.499999999999996447, 1.469576158976823947E-15 ) ) ;
#2425 = ORIENTED_EDGE ( 'NONE', *, *, #13673, .F. ) ;
#2426 = DIRECTION ( 'NONE',  ( 0.000000000000000000, 0.000000000000000000, 1.000000000000000000 ) ) ;
#2427 = EDGE_CURVE ( 'NONE', #22344, #3030, #8546, .T. ) ;
#2428 = CARTESIAN_POINT ( 'NONE',  ( -10.38193264731104648, 30.83255023748043655, 43.52061562521062399 ) ) ;
#2429 = CARTESIAN_POINT ( 'NONE',  ( -9.999999999999758415, -3.000000000000169198, -4.999999999999984013 ) ) ;
#2430 = CIRCLE ( 'NONE', #4262, 1.000000000000000888 ) ;
#2431 = AXIS2_PLACEMENT_3D ( 'NONE', #11425, #7878, #7759 ) ;
#2432 = AXIS2_PLACEMENT_3D ( 'NONE', #10888, #7346, #15812 ) ;
#2433 = EDGE_CURVE ( 'NONE', #17903, #10299, #3295, .T. ) ;
#2434 = EDGE_LOOP ( 'NONE', ( #8528, #1302, #8110, #3876 ) ) ;
#2435 = AXIS2_PLACEMENT_3D ( 'NONE', #3194, #11770, #3075 ) ;
#2436 = EDGE_LOOP ( 'NONE', ( #20453, #6374, #6252, #19334 ) ) ;
#2437 = ORIENTED_EDGE ( 'NONE', *, *, #11521, .T. ) ;
#2438 = DIRECTION ( 'NONE',  ( 0.1436291612043040788, 0.9896287191852403131, 0.002379541033241383378 ) ) ;
#2439 = ORIENTED_EDGE ( 'NONE', *, *, #14768, .T. ) ;
#2440 = DIRECTION ( 'NONE',  ( 6.505213034913038160E-19, 3.903127820947822896E-18, 1.000000000000000000 ) ) ;
#2441 = DIRECTION ( 'NONE',  ( 1.000000000000000000, 0.000000000000000000, 0.000000000000000000 ) ) ;
#2442 =( REPRESENTATION_RELATIONSHIP ('NONE','NONE', #8442, #15726 ) REPRESENTATION_RELATIONSHIP_WITH_TRANSFORMATION ( #3681 )SHAPE_REPRESENTATION_RELATIONSHIP( ) );
#2443 = FACE_OUTER_BOUND ( 'NONE', #20008, .T. ) ;
#2444 = CARTESIAN_POINT ( 'NONE',  ( 34.99999999999980815, 28.00000000000000000, 57.49999999999921840 ) ) ;
#2445 = CARTESIAN_POINT ( 'NONE',  ( 42.50000000000000711, -12.00000000000012434, 50.02500000000011937 ) ) ;
#2446 = ORIENTED_EDGE ( 'NONE', *, *, #3743, .F. ) ;
#2447 = LINE ( 'NONE', #19860, #304 ) ;
#2448 = CARTESIAN_POINT ( 'NONE',  ( 28.95348479018572263, -14.76298474240511638, -6.999999999999999112 ) ) ;
#2449 = ORIENTED_EDGE ( 'NONE', *, *, #5012, .F. ) ;
#2450 = CARTESIAN_POINT ( 'NONE',  ( 21.05198877411804048, -30.13956425491232238, 2.800654218530485018 ) ) ;
#2451 = CARTESIAN_POINT ( 'NONE',  ( 1.110223024625156540E-13, -5.551115123125782702E-14, -6.999999999999950262 ) ) ;
#2452 = DIRECTION ( 'NONE',  ( -6.505213034913038160E-19, -3.903127820947822896E-18, -1.000000000000000000 ) ) ;
#2453 = EDGE_LOOP ( 'NONE', ( #11507, #15045, #19659, #10420 ) ) ;
#2454 = LINE ( 'NONE', #11259, #17473 ) ;
#2455 = LINE ( 'NONE', #736, #7262 ) ;
#2456 = ORIENTED_EDGE ( 'NONE', *, *, #21678, .T. ) ;
#2457 = CARTESIAN_POINT ( 'NONE',  ( 6.803227178529145824, 38.81166136533732214, 55.43135129401766648 ) ) ;
#2458 = CARTESIAN_POINT ( 'NONE',  ( -34.99999999999999289, 0.000000000000000000, -3.012171160963566127E-14 ) ) ;
#2459 = CARTESIAN_POINT ( 'NONE',  ( -17.09029715894932977, 27.64365646977273627, -6.999999999999999112 ) ) ;
#2460 = ORIENTED_EDGE ( 'NONE', *, *, #10047, .T. ) ;
#2461 = ADVANCED_FACE ( 'NONE', ( #22423 ), #685, .F. ) ;
#2462 = DIRECTION ( 'NONE',  ( 0.000000000000000000, -0.000000000000000000, 1.000000000000000000 ) ) ;
#2463 = CARTESIAN_POINT ( 'NONE',  ( 18.22261011550299514, 31.92986134326217140, -2.800654218530460593 ) ) ;
#2464 = DIRECTION ( 'NONE',  ( 8.659560562354982162E-17, 0.7071067811865435759, -0.7071067811865515695 ) ) ;
#2465 = AXIS2_PLACEMENT_3D ( 'NONE', #17422, #17, #20762 ) ;
#2466 = EDGE_CURVE ( 'NONE', #13970, #20079, #12744, .T. ) ;
#2467 = EDGE_CURVE ( 'NONE', #2631, #2388, #19331, .T. ) ;
#2468 = VECTOR ( 'NONE', #5542, 1000.000000000000000 ) ;
#2470 = EDGE_CURVE ( 'NONE', #5472, #3556, #22295, .T. ) ;
#2469 = EDGE_LOOP ( 'NONE', ( #13082, #11885 ) ) ;
#2471 = EDGE_LOOP ( 'NONE', ( #2738, #11209 ) ) ;
#2472 = VERTEX_POINT ( 'NONE', #1559 ) ;
#2473 = VERTEX_POINT ( 'NONE', #17595 ) ;
#2474 = CYLINDRICAL_SURFACE ( 'NONE', #16918, 15.00000000000000000 ) ;
#2475 = CYLINDRICAL_SURFACE ( 'NONE', #21721, 12.00000000000000000 ) ;
#2476 = DIRECTION ( 'NONE',  ( 0.000000000000000000, 0.7071067811865721087, 0.7071067811865230368 ) ) ;
#2477 = VERTEX_POINT ( 'NONE', #10698 ) ;
#2478 = DIRECTION ( 'NONE',  ( 0.000000000000000000, 0.000000000000000000, -1.000000000000000000 ) ) ;
#2479 = CIRCLE ( 'NONE', #11987, 2.500000000000002220 ) ;
#2480 = VERTEX_POINT ( 'NONE', #13683 ) ;
#2481 = FACE_OUTER_BOUND ( 'NONE', #14323, .T. ) ;
#2482 = VECTOR ( 'NONE', #1567, 1000.000000000000114 ) ;
#2483 = CARTESIAN_POINT ( 'NONE',  ( -9.689843208404459673, 39.33333333333334991, -54.54983754392748807 ) ) ;
#2484 = CYLINDRICAL_SURFACE ( 'NONE', #16671, 59.99999999999703704 ) ;
#2485 = AXIS2_PLACEMENT_3D ( 'NONE', #6864, #20850, #13709 ) ;
#2486 = CARTESIAN_POINT ( 'NONE',  ( 35.00000000000000000, 25.00000000000000000, 4.258610482196280173E-15 ) ) ;
#2487 = DIRECTION ( 'NONE',  ( 0.000000000000000000, 0.5150380749100562650, 0.8571673007021111124 ) ) ;
#2488 = DIRECTION ( 'NONE',  ( 9.523972024970703335E-16, 0.000000000000000000, 1.000000000000000000 ) ) ;
#2489 = AXIS2_PLACEMENT_3D ( 'NONE', #175, #18139, #1908 ) ;
#2490 = DIRECTION ( 'NONE',  ( -0.4332438415859253822, 0.000000000000000000, 0.9012767464701779696 ) ) ;
#2491 = EDGE_LOOP ( 'NONE', ( #16736, #17445, #19403, #21173 ) ) ;
#2492 = VECTOR ( 'NONE', #4133, 1000.000000000000000 ) ;
#2493 = ORIENTED_EDGE ( 'NONE', *, *, #14262, .T. ) ;
#2494 = AXIS2_PLACEMENT_3D ( 'NONE', #6744, #17162, #8461 ) ;
#2495 = ADVANCED_FACE ( 'NONE', ( #8663 ), #11827, .T. ) ;
#2496 = ORIENTED_EDGE ( 'NONE', *, *, #213, .F. ) ;
#2497 = CARTESIAN_POINT ( 'NONE',  ( 4.044183821322609990E-15, 3.000000000000006217, 0.000000000000000000 ) ) ;
#2498 = EDGE_CURVE ( 'NONE', #312, #5560, #12650, .T. ) ;
#2499 = CYLINDRICAL_SURFACE ( 'NONE', #3959, 31.50000000000001421 ) ;
#2500 = AXIS2_PLACEMENT_3D ( 'NONE', #5716, #14639, #10983 ) ;
#2501 = EDGE_CURVE ( 'NONE', #15970, #12342, #4312, .T. ) ;
#2502 = DIRECTION ( 'NONE',  ( 0.000000000000000000, 1.000000000000000000, 0.000000000000000000 ) ) ;
#2503 = DIRECTION ( 'NONE',  ( -0.000000000000000000, -1.000000000000000000, -0.000000000000000000 ) ) ;
#2504 = CARTESIAN_POINT ( 'NONE',  ( 0.7809641287214827976, -4.625293788890135538, 46.06432795380052170 ) ) ;
#2505 = CARTESIAN_POINT ( 'NONE',  ( -35.00000000000058265, 40.00000000000000000, -55.00000000000076028 ) ) ;
#2506 = FILL_AREA_STYLE_COLOUR ( '', #13846 ) ;
#2507 = DIRECTION ( 'NONE',  ( -1.000000000000000000, 1.567804759296643123E-16, 0.000000000000000000 ) ) ;
#2508 = VECTOR ( 'NONE', #13892, 1000.000000000000000 ) ;
#2509 = CIRCLE ( 'NONE', #8007, 31.50000000000000711 ) ;
#2510 = ORIENTED_EDGE ( 'NONE', *, *, #3448, .F. ) ;
#2511 = VECTOR ( 'NONE', #20802, 1000.000000000000000 ) ;
#2512 = CARTESIAN_POINT ( 'NONE',  ( 25.99999999999998579, 19.99999999999999645, -105.0000000000000142 ) ) ;
#2513 = CARTESIAN_POINT ( 'NONE',  ( -35.00000000000000000, 22.00000000000000711, 2.255140518769849223E-14 ) ) ;
#2514 = DIRECTION ( 'NONE',  ( -1.000000000000000000, 0.000000000000000000, -0.000000000000000000 ) ) ;
#2515 = DIRECTION ( 'NONE',  ( 1.000000000000000000, 0.000000000000000000, 0.000000000000000000 ) ) ;
#2516 = CONICAL_SURFACE ( 'NONE', #1785, 2.099999999999997868, 1.029744258676652091 ) ;
#2517 = VERTEX_POINT ( 'NONE', #21610 ) ;
#2518 = CARTESIAN_POINT ( 'NONE',  ( 4.025500340002624355, -36.54278193890314697, 2.800654218530485018 ) ) ;
#2519 = CARTESIAN_POINT ( 'NONE',  ( -17.66631876130915657, 31.41173278719225337, -6.999999999999950262 ) ) ;
#2520 = LINE ( 'NONE', #4463, #14838 ) ;
#2521 = AXIS2_PLACEMENT_3D ( 'NONE', #13809, #20827, #22206 ) ;
#2522 = VECTOR ( 'NONE', #1394, 1000.000000000000000 ) ;
#2523 = ORIENTED_EDGE ( 'NONE', *, *, #16926, .T. ) ;
#2524 = CARTESIAN_POINT ( 'NONE',  ( -42.50000000000000711, -5.000000000000000000, -47.50000000000000000 ) ) ;
#2525 = CARTESIAN_POINT ( 'NONE',  ( 7.130216064151039923, 40.00000000000000000, -52.60396709977539587 ) ) ;
#2526 = TOROIDAL_SURFACE ( 'NONE', #309, 34.90673715956759082, 8.750000000000000000 ) ;
#2527 = ORIENTED_EDGE ( 'NONE', *, *, #17266, .T. ) ;
#2528 = CARTESIAN_POINT ( 'NONE',  ( 3.658198312395513518, 39.91812900842233347, -51.36232427839211567 ) ) ;
#2529 = DIRECTION ( 'NONE',  ( 0.000000000000000000, 0.000000000000000000, 1.000000000000000000 ) ) ;
#2530 = ORIENTED_EDGE ( 'NONE', *, *, #6684, .T. ) ;
#2531 = CARTESIAN_POINT ( 'NONE',  ( 2.220446049250313081E-13, 2.775557561562891351E-14, -2.800654218530485018 ) ) ;
#2532 = DIRECTION ( 'NONE',  ( -0.000000000000000000, 1.000000000000000000, -0.000000000000000000 ) ) ;
#2533 = LINE ( 'NONE', #15094, #14889 ) ;
#2534 = DIRECTION ( 'NONE',  ( -1.000000000000000000, -1.208970125616077665E-17, 0.000000000000000000 ) ) ;
#2535 = CYLINDRICAL_SURFACE ( 'NONE', #2656, 36.76383501243555685 ) ;
#2536 = AXIS2_PLACEMENT_3D ( 'NONE', #10267, #6850, #10490 ) ;
#2537 = ORIENTED_EDGE ( 'NONE', *, *, #19117, .F. ) ;
#2538 = DIRECTION ( 'NONE',  ( -0.000000000000000000, 1.000000000000000000, -0.000000000000000000 ) ) ;
#2539 = DIRECTION ( 'NONE',  ( -0.000000000000000000, -0.000000000000000000, 1.000000000000000000 ) ) ;
#2540 = AXIS2_PLACEMENT_3D ( 'NONE', #3716, #1983, #258 ) ;
#2541 = CARTESIAN_POINT ( 'NONE',  ( -1.387778780781445518E-14, 20.00000000000000355, 102.0000000000000142 ) ) ;
#2542 = ADVANCED_FACE ( 'NONE', ( #14365 ), #14252, .F. ) ;
#2543 = ORIENTED_EDGE ( 'NONE', *, *, #8775, .F. ) ;
#2544 = CARTESIAN_POINT ( 'NONE',  ( 8.349099696857495090, 1.803277857257809424, 53.93591755799672427 ) ) ;
#2545 = DIRECTION ( 'NONE',  ( -1.000000000000000000, 0.000000000000000000, 0.000000000000000000 ) ) ;
#2546 = AXIS2_PLACEMENT_3D ( 'NONE', #11588, #13274, #8044 ) ;
#2547 = ADVANCED_FACE ( 'NONE', ( #8998 ), #10944, .T. ) ;
#2548 = PRODUCT ( 'FRONT COVER', 'FRONT COVER', '', ( #6769 ) ) ;
#2549 = EDGE_LOOP ( 'NONE', ( #4013, #10589, #21393, #55, #10631 ) ) ;
#2550 = ORIENTED_EDGE ( 'NONE', *, *, #1258, .T. ) ;
#2551 = VECTOR ( 'NONE', #2850, 1000.000000000000000 ) ;
#2552 = ORIENTED_EDGE ( 'NONE', *, *, #10261, .T. ) ;
#2553 = UNCERTAINTY_MEASURE_WITH_UNIT (LENGTH_MEASURE( 1.000000000000000082E-05 ), #19676, 'distance_accuracy_value', 'NONE');
#2554 = ORIENTED_EDGE ( 'NONE', *, *, #9741, .F. ) ;
#2555 = LINE ( 'NONE', #820, #5193 ) ;
#2556 = CARTESIAN_POINT ( 'NONE',  ( 7.480086125706187694, -0.2526605362868768467, 53.02285530597295349 ) ) ;
#2557 = DIRECTION ( 'NONE',  ( 0.000000000000000000, -1.000000000000000000, 0.000000000000000000 ) ) ;
#2558 = CARTESIAN_POINT ( 'NONE',  ( 24.79619811426236708, -21.00948735876897899, 3.000000000000016431 ) ) ;
#2559 = DIRECTION ( 'NONE',  ( -1.000000000000000000, 0.000000000000000000, 0.000000000000000000 ) ) ;
#2560 = VERTEX_POINT ( 'NONE', #5909 ) ;
#2561 = DIRECTION ( 'NONE',  ( -0.000000000000000000, -1.000000000000000000, -0.000000000000000000 ) ) ;
#2562 = CARTESIAN_POINT ( 'NONE',  ( 6.696867368503558448E-15, 40.00000000000000000, 48.73397172404481381 ) ) ;
#2563 = VERTEX_POINT ( 'NONE', #2241 ) ;
#2564 = CARTESIAN_POINT ( 'NONE',  ( -34.99999999999999289, 0.000000000000000000, -57.49999999999705125 ) ) ;
#2565 = FACE_OUTER_BOUND ( 'NONE', #16556, .T. ) ;
#2566 = CARTESIAN_POINT ( 'NONE',  ( 14.04165170564756870, 5.752764646445603702, -58.83649392397241229 ) ) ;
#2567 = EDGE_LOOP ( 'NONE', ( #11959, #4394, #19309, #6880 ) ) ;
#2568 = LINE ( 'NONE', #18257, #2055 ) ;
#2569 = CARTESIAN_POINT ( 'NONE',  ( 22.15900668633785742, 29.33526866242092268, -1.999999999999991340 ) ) ;
#2570 = VERTEX_POINT ( 'NONE', #21719 ) ;
#2571 = ADVANCED_FACE ( 'NONE', ( #12989 ), #9225, .T. ) ;
#2572 = DIRECTION ( 'NONE',  ( 0.000000000000000000, 0.000000000000000000, -1.000000000000000000 ) ) ;
#2573 = CARTESIAN_POINT ( 'NONE',  ( -8.349099696861340902, 1.803277857259562911, -53.93591755799872800 ) ) ;
#2574 = ORIENTED_EDGE ( 'NONE', *, *, #9619, .T. ) ;
#2575=STYLED_ITEM('',(#22748),#18432);
#2576 = CARTESIAN_POINT ( 'NONE',  ( 21.69710536060296135, 28.14364593009908688, 3.000000000000044853 ) ) ;
#2577 = LINE ( 'NONE', #12863, #832 ) ;
#2578 = CARTESIAN_POINT ( 'NONE',  ( 11.59291124596733091, 39.24500985575833312, -55.27372209264543557 ) ) ;
#2579 = B_SPLINE_CURVE_WITH_KNOTS ( 'NONE', 3,
 ( #2217, #17798, #9094, #3614, #10574, #17572, #19520, #15833, #5430, #12409, #3720, #7260, #3828, #16072, #380, #7373, #5646, #12620, #19639, #3943, #16177, #20092, #11486, #12965, #18473, #19976, #6110, #9771, #731, #7712, #21931, #14577, #4507, #9320, #12850, #11256, #9653, #18254 ),
 .UNSPECIFIED., .F., .F.,
 ( 4, 2, 2, 2, 2, 2, 2, 2, 2, 2, 2, 2, 2, 2, 2, 2, 2, 2, 4 ),
 ( 0.002265996298495699668, 0.003649092030476641657, 0.005032187762457583646, 0.007798379226419466757, 0.01056457069038134813, 0.01333076215434323038, 0.01609695361830511262, 0.01886314508226699313, 0.02439552801019075068, 0.02577862374217168920, 0.02716171947415263466, 0.02992791093811452557, 0.03131100667009547450, 0.03269410240207642343, 0.03546029386603831435, 0.03822648533000020526, 0.03960958106198115419, 0.04099267679396210312, 0.04652505972188589189 ),
 .UNSPECIFIED. ) ;
#2580 = VERTEX_POINT ( 'NONE', #9347 ) ;
#2581 = AXIS2_PLACEMENT_3D ( 'NONE', #3232, #5500, #15908 ) ;
#2582 = VERTEX_POINT ( 'NONE', #16204 ) ;
#2583 = ORIENTED_EDGE ( 'NONE', *, *, #2335, .F. ) ;
#2584 = ORIENTED_EDGE ( 'NONE', *, *, #9100, .F. ) ;
#2585 = FACE_OUTER_BOUND ( 'NONE', #17532, .T. ) ;
#2586 = DIRECTION ( 'NONE',  ( -1.000000000000000000, 0.000000000000000000, 1.445602896647339163E-16 ) ) ;
#2587 = PLANE ( 'NONE',  #8818 ) ;
#2588 = ADVANCED_FACE ( 'NONE', ( #9466 ), #19884, .F. ) ;
#2589 = ORIENTED_EDGE ( 'NONE', *, *, #4315, .F. ) ;
#2590 = DIRECTION ( 'NONE',  ( 0.000000000000000000, 0.000000000000000000, -1.000000000000000000 ) ) ;
#2591 = FACE_OUTER_BOUND ( 'NONE', #7850, .T. ) ;
#2592 = ORIENTED_EDGE ( 'NONE', *, *, #16916, .F. ) ;
#2593 = VERTEX_POINT ( 'NONE', #19782 ) ;
#2594 = CARTESIAN_POINT ( 'NONE',  ( -6.041077103370482426, -0.8288449397156264498, -52.13906252460640900 ) ) ;
#2595 = CARTESIAN_POINT ( 'NONE',  ( 2.999999999999998668, 22.79878727884707956, 8.485281374238567764 ) ) ;
#2596 = EDGE_CURVE ( 'NONE', #14190, #8015, #20812, .T. ) ;
#2597 = FACE_OUTER_BOUND ( 'NONE', #9543, .T. ) ;
#2598 = ADVANCED_FACE ( 'NONE', ( #16330 ), #20004, .F. ) ;
#2599 = FACE_OUTER_BOUND ( 'NONE', #1818, .T. ) ;
#2600 = AXIS2_PLACEMENT_3D ( 'NONE', #4769, #11738, #9684 ) ;
#2601 = CARTESIAN_POINT ( 'NONE',  ( -8.999999999999841904, -5.551115123125782702E-14, 5.000000000000022204 ) ) ;
#2602 = LINE ( 'NONE', #870, #15961 ) ;
#2603 = ADVANCED_FACE ( 'NONE', ( #17822 ), #21265, .F. ) ;
#2604 = ORIENTED_EDGE ( 'NONE', *, *, #20625, .T. ) ;
#2605 = ORIENTED_EDGE ( 'NONE', *, *, #14981, .F. ) ;
#2606 = B_SPLINE_CURVE_WITH_KNOTS ( 'NONE', 3,
 ( #12871, #19880, #5454, #8994 ),
 .UNSPECIFIED., .F., .F.,
 ( 4, 4 ),
 ( 9.545285769294494988E-07, 0.001900595205834635293 ),
 .UNSPECIFIED. ) ;
#2607 = EDGE_CURVE ( 'NONE', #14950, #4040, #6765, .T. ) ;
#2608 = ORIENTED_EDGE ( 'NONE', *, *, #10655, .F. ) ;
#2609 = CARTESIAN_POINT ( 'NONE',  ( -20.32373648405383193, 10.46972314276651872, 58.17772014969900596 ) ) ;
#2610 = FACE_BOUND ( 'NONE', #18350, .T. ) ;
#2611 = VECTOR ( 'NONE', #4531, 1000.000000000000000 ) ;
#2612 = EDGE_CURVE ( 'NONE', #10824, #5940, #858, .T. ) ;
#2613 = B_SPLINE_CURVE_WITH_KNOTS ( 'NONE', 3,
 ( #12709, #19730, #11001, #9286 ),
 .UNSPECIFIED., .F., .F.,
 ( 4, 4 ),
 ( 9.715086411615364248E-07, 0.001929643240672571482 ),
 .UNSPECIFIED. ) ;
#2614 = CARTESIAN_POINT ( 'NONE',  ( 17.09029715894957846, -27.64365646977279312, -2.999999999999992450 ) ) ;
#2615 = CARTESIAN_POINT ( 'NONE',  ( -8.646032897229122938, 31.21605069118058040, -2.999999999999957367 ) ) ;
#2616 = B_SPLINE_CURVE_WITH_KNOTS ( 'NONE', 3,
 ( #15225, #20300, #7800, #16510 ),
 .UNSPECIFIED., .F., .F.,
 ( 4, 4 ),
 ( 9.715086408138421055E-07, 0.001929643240672349221 ),
 .UNSPECIFIED. ) ;
#2617 = CARTESIAN_POINT ( 'NONE',  ( -5.833333333333325932, 39.00000000000000711, 40.61164310337068883 ) ) ;
#2618 = CARTESIAN_POINT ( 'NONE',  ( -3.499474518498425473E-16, -0.4099377891817043151, 48.99242580662814106 ) ) ;
#2619 = CARTESIAN_POINT ( 'NONE',  ( -34.99999999999980815, 26.00000000000000355, 52.89999999999922409 ) ) ;
#2620 = CARTESIAN_POINT ( 'NONE',  ( -7.938322399558154885, 38.36220367130613340, -56.16250688146275394 ) ) ;
#2621 = EDGE_CURVE ( 'NONE', #11042, #7992, #9766, .T. ) ;
#2622 = DIRECTION ( 'NONE',  ( -6.505213034913038160E-19, -3.903127820947822896E-18, -1.000000000000000000 ) ) ;
#2623 = CARTESIAN_POINT ( 'NONE',  ( -35.00000000000058265, 40.00000000000000000, -52.90000000000076597 ) ) ;
#2624 = CIRCLE ( 'NONE', #1525, 2.099999999999990763 ) ;
#2625 = ORIENTED_EDGE ( 'NONE', *, *, #16777, .F. ) ;
#2626 = CARTESIAN_POINT ( 'NONE',  ( -35.00000000000000000, 40.00000000000000000, 1.387778780781445676E-14 ) ) ;
#2627 = DIRECTION ( 'NONE',  ( 6.505213034913038160E-19, 3.903127820947822896E-18, 1.000000000000000000 ) ) ;
#2628 = LINE ( 'NONE', #7428, #17740 ) ;
#2629 = DIRECTION ( 'NONE',  ( 0.000000000000000000, 0.000000000000000000, 1.000000000000000000 ) ) ;
#2630 = EDGE_CURVE ( 'NONE', #3259, #22398, #13450, .T. ) ;
#2631 = VERTEX_POINT ( 'NONE', #6136 ) ;
#2632 = FACE_BOUND ( 'NONE', #15399, .T. ) ;
#2633 = DIRECTION ( 'NONE',  ( -1.000000000000000000, 0.000000000000000000, 0.000000000000000000 ) ) ;
#2634 = DIRECTION ( 'NONE',  ( -1.000000000000000000, 1.070969311094961116E-14, 0.000000000000000000 ) ) ;
#2635 = DIRECTION ( 'NONE',  ( 0.000000000000000000, 0.000000000000000000, -1.000000000000000000 ) ) ;
#2636 = EDGE_CURVE ( 'NONE', #575, #6067, #20441, .T. ) ;
#2637 = EDGE_CURVE ( 'NONE', #16920, #5292, #18981, .T. ) ;
#2638 = EDGE_LOOP ( 'NONE', ( #1975, #18570 ) ) ;
#2639 = DIRECTION ( 'NONE',  ( 1.000000000000000000, 0.000000000000000000, 0.000000000000000000 ) ) ;
#2640 = CARTESIAN_POINT ( 'NONE',  ( -13.85640646055084702, -25.00000000000000000, 7.999999999999705125 ) ) ;
#2641 = ORIENTED_EDGE ( 'NONE', *, *, #12470, .F. ) ;
#2642 = CARTESIAN_POINT ( 'NONE',  ( 3.000000000000000444, 15.20112712106396913, 8.485281374238567764 ) ) ;
#2643 = PLANE ( 'NONE',  #3678 ) ;
#2644 = CARTESIAN_POINT ( 'NONE',  ( -9.708269511265104512, 33.52953626616034200, -2.999999999999978240 ) ) ;
#2645 = DIRECTION ( 'NONE',  ( -1.000000000000000000, 0.000000000000000000, 0.000000000000000000 ) ) ;
#2646 = CARTESIAN_POINT ( 'NONE',  ( -12.27586057105639838, 4.193657236093905283, -55.54740530680978594 ) ) ;
#2647 = DIRECTION ( 'NONE',  ( -6.505213034913038160E-19, -3.903127820947822896E-18, -1.000000000000000000 ) ) ;
#2648 = CARTESIAN_POINT ( 'NONE',  ( -90.00000000000000000, 40.00000000000000711, -9.108981535246192915E-16 ) ) ;
#2649 = ORIENTED_EDGE ( 'NONE', *, *, #12103, .F. ) ;
#2650 = CARTESIAN_POINT ( 'NONE',  ( 6.742883674876798850, 34.24928931925757780, -2.999999999999971578 ) ) ;
#2651 = DIRECTION ( 'NONE',  ( 0.000000000000000000, -1.000000000000000000, 0.000000000000000000 ) ) ;
#2652 = FACE_OUTER_BOUND ( 'NONE', #3675, .T. ) ;
#2653 = EDGE_CURVE ( 'NONE', #14416, #22631, #5060, .T. ) ;
#2654 = ORIENTED_EDGE ( 'NONE', *, *, #13007, .T. ) ;
#2655 = CARTESIAN_POINT ( 'NONE',  ( 8.923978417719926171, 2.083761144193561066, 56.51262908347950997 ) ) ;
#2656 = AXIS2_PLACEMENT_3D ( 'NONE', #13260, #18445, #2759 ) ;
#2657 = CARTESIAN_POINT ( 'NONE',  ( 3.469446951953614189E-15, 6.776263578034402713E-17, 18.00000000000000711 ) ) ;
#2658 = CARTESIAN_POINT ( 'NONE',  ( -36.06598984771573413, 10.00000000000000000, 48.42385786802029912 ) ) ;
#2659 = EDGE_CURVE ( 'NONE', #6902, #13173, #9095, .T. ) ;
#2660 = EDGE_LOOP ( 'NONE', ( #6265, #17790, #11522, #5448 ) ) ;
#2661 = ORIENTED_EDGE ( 'NONE', *, *, #17816, .F. ) ;
#2662 = B_SPLINE_CURVE_WITH_KNOTS ( 'NONE', 3,
 ( #21325, #21563, #1964, #240, #19842, #19498, #2193, #7459, #10890, #12484, #7119, #17892, #5621, #17998, #12597, #12387, #16049, #3803, #10649, #8948, #9295, #7235, #4143, #11011, #15813, #2302, #21106, #19395, #11119, #2077, #18109, #8838, #3700, #16151, #19611, #123, #14204, #10765, #21216, #14431, #17771, #14316, #464, #585, #14552, #9071, #21440, #358, #7348, #5743, #4043, #16274, #7573, #5862, #20407, #4258, #707, #11691, #15103, #16505, #14994, #11351, #21905, #4375, #6201, #13164, #20067, #812, #18336, #4482, #2881, #1149 ),
 .UNSPECIFIED., .F., .F.,
 ( 4, 2, 1, 2, 2, 1, 1, 2, 2, 2, 2, 1, 1, 1, 1, 1, 2, 2, 2, 1, 1, 1, 1, 1, 2, 2, 1, 1, 1, 1, 2, 2, 1, 1, 2, 2, 1, 2, 2, 2, 1, 1, 2, 2, 2, 2, 4 ),
 ( 0.000000000000000000, 0.2499923706055057759, 0.2812414169311941992, 0.2851475477219057586, 0.2871006131172617604, 0.2890536785126177621, 0.2968659400940392712, 0.3124904632568824558, 0.3749885559082549724, 0.4999847412109998945, 0.5019378066063551191, 0.5038908720017102327, 0.5077970027924207930, 0.5156092643738410253, 0.5312337875366800466, 0.5624828338623590884, 0.6249809265137173941, 0.7499771118164337835, 0.7519301772117895633, 0.7538832426071453430, 0.7577893733978569024, 0.7656016349792786890, 0.7812261581421213741, 0.8124752044678077434, 0.8749732971191792608, 0.8769263625145349295, 0.8788794279098904871, 0.8827855587006018245, 0.8905978202820242773, 0.9062223434448704040, 0.9374713897705615473, 0.9413775205612727737, 0.9452836513519840000, 0.9530959129334075630, 0.9687204360962549110, 0.9726265668869673586, 0.9765326976776796952, 0.9843449592591031472, 0.9921572208405267101, 0.9926454871893649612, 0.9931337535382033233, 0.9941102862358790482, 0.9960633516312306091, 0.9965516179800615326, 0.9970398843288925672, 0.9980164170265533041, 0.9999694824218750000 ),
 .UNSPECIFIED. ) ;
#2663 = ADVANCED_FACE ( 'NONE', ( #20119 ), #6588, .F. ) ;
#2664 = ORIENTED_EDGE ( 'NONE', *, *, #14038, .T. ) ;
#2665 = CARTESIAN_POINT ( 'NONE',  ( 12.24744603029285273, 40.00000000000000000, 54.43639671998466412 ) ) ;
#2666 = DIRECTION ( 'NONE',  ( 6.505213034913038160E-19, 3.903127820947822896E-18, 1.000000000000000000 ) ) ;
#2667 = AXIS2_PLACEMENT_3D ( 'NONE', #10055, #4811, #22578 ) ;
#2668 = CONICAL_SURFACE ( 'NONE', #8144, 2.099999999999990763, 1.029744258676652091 ) ;
#2669 = DIRECTION ( 'NONE',  ( 4.718764931986839378E-35, -3.903127820947822896E-18, -1.000000000000000000 ) ) ;
#2670 = CARTESIAN_POINT ( 'NONE',  ( -22.00000000000001421, 20.00000000000000355, 100.0000000000000000 ) ) ;
#2671 = CARTESIAN_POINT ( 'NONE',  ( -2.783226368218592341E-14, 0.000000000000000000, 47.49736834814792985 ) ) ;
#2672 = ORIENTED_EDGE ( 'NONE', *, *, #10261, .F. ) ;
#2673 = FACE_OUTER_BOUND ( 'NONE', #3912, .T. ) ;
#2674 = ORIENTED_EDGE ( 'NONE', *, *, #17086, .T. ) ;
#2675 = AXIS2_PLACEMENT_3D ( 'NONE', #5443, #19768, #19533 ) ;
#2676 = DIRECTION ( 'NONE',  ( 0.000000000000000000, 0.000000000000000000, 1.000000000000000000 ) ) ;
#2677 = ADVANCED_FACE ( 'NONE', ( #13104 ), #1194, .T. ) ;
#2678 = DIRECTION ( 'NONE',  ( 0.000000000000000000, 0.000000000000000000, 1.000000000000000000 ) ) ;
#2679 = ORIENTED_EDGE ( 'NONE', *, *, #3365, .T. ) ;
#2680 = FACE_OUTER_BOUND ( 'NONE', #22269, .T. ) ;
#2681 = CARTESIAN_POINT ( 'NONE',  ( 5.666031183648402525, 39.18449859167989757, -54.55698311759260122 ) ) ;
#2682 = ORIENTED_EDGE ( 'NONE', *, *, #19566, .T. ) ;
#2683 = DIRECTION ( 'NONE',  ( -1.000000000000000000, 1.530638361156006245E-16, 0.000000000000000000 ) ) ;
#2684 = CARTESIAN_POINT ( 'NONE',  ( -3.711215864303547551, -1.139709857517552605, -50.71371062340998037 ) ) ;
#2685 = ORIENTED_EDGE ( 'NONE', *, *, #6152, .T. ) ;
#2686 = DIRECTION ( 'NONE',  ( 0.000000000000000000, 1.000000000000000000, 0.000000000000000000 ) ) ;
#2687 = CARTESIAN_POINT ( 'NONE',  ( 24.62019382530528233, -4.341204441673129466, 3.000000000000023537 ) ) ;
#2688 = DIRECTION ( 'NONE',  ( 0.000000000000000000, 0.000000000000000000, 1.000000000000000000 ) ) ;
#2689 = VECTOR ( 'NONE', #2724, 1000.000000000000000 ) ;
#2690 = CARTESIAN_POINT ( 'NONE',  ( 20.11496009237018256, 10.03305173526324445, -58.12476682723747956 ) ) ;
#2691 = CIRCLE ( 'NONE', #502, 0.9999999999999974465 ) ;
#2692 = VERTEX_POINT ( 'NONE', #15043 ) ;
#2693 = VERTEX_POINT ( 'NONE', #15154 ) ;
#2694 = VERTEX_POINT ( 'NONE', #13550 ) ;
#2695 = ADVANCED_FACE ( 'NONE', ( #13208 ), #4422, .F. ) ;
#2696 = EDGE_LOOP ( 'NONE', ( #10369, #9322, #10556, #3613 ) ) ;
#2697 = CARTESIAN_POINT ( 'NONE',  ( 30.13956425491251423, 21.05198877411795877, -1.999999999999953149 ) ) ;
#2698 = CARTESIAN_POINT ( 'NONE',  ( 12.99999999999999467, 20.00000000000000000, 11.32475165290614960 ) ) ;
#2699 =( BOUNDED_SURFACE ( )  B_SPLINE_SURFACE ( 3, 2, ( 
 ( #20266, #7888, #3390 ),
 ( #4572, #14852, #15188 ),
 ( #4457, #22213, #11547 ),
 ( #9714, #21876, #20806 ),
 ( #10349, #17351, #8650 ),
 ( #15625, #13139, #20153 ),
 ( #10926, #5779, #14349 ),
 ( #10805, #3839, #9210 ),
 ( #21477, #7274, #12756 ),
 ( #15842, #19429, #389 ),
 ( #17810, #19767, #274 ),
 ( #7384, #12518, #1787 ),
 ( #52, #21360, #19315 ),
 ( #10681, #5658, #21252 ),
 ( #15740, #498, #7042 ),
 ( #8982, #14236, #15963 ),
 ( #5543, #17688, #7497 ),
 ( #3624, #21140, #4072 ),
 ( #3729, #19532, #17465 ),
 ( #16188, #8771, #12633 ),
 ( #2114, #14466, #9106 ),
 ( #10583, #14001, #16082 ),
 ( #21029, #19652, #17582 ),
 ( #3957, #17923, #2227 ),
 ( #5330, #12310, #1889 ),
 ( #8871, #155, #7149 ),
 ( #14120, #5442, #12417 ),
 ( #2000, #13304, #9556 ),
 ( #11381, #21597, #21705 ),
 ( #13193, #15029, #6004 ),
 ( #9666, #6121, #7723 ),
 ( #9331, #9781, #20328 ),
 ( #14696, #2340, #16310 ),
 ( #6237, #16773, #16541 ),
 ( #4519, #843, #7955 ),
 ( #12975, #6340, #19989 ),
 ( #7833, #11039, #16653 ),
 ( #22047, #21943, #18027 ) ),
 .UNSPECIFIED., .F., .F., .F. ) 
 B_SPLINE_SURFACE_WITH_KNOTS ( ( 4, 2, 2, 2, 2, 2, 2, 2, 2, 2, 2, 2, 2, 2, 2, 2, 2, 2, 4 ),
 ( 3, 3 ),
 ( 0.000000000000000000, 0.005809515383400559035, 0.008714273075100838553, 0.01161903076680111807, 0.01452378845850139759, 0.01742854615020167711, 0.02033330384190195489, 0.02178568268775209552, 0.02323806153360223614, 0.02614281922530251739, 0.02759519807115265455, 0.02904757691700279518, 0.03485709230040335421, 0.03630947114625349137, 0.03776184999210363546, 0.04066660768380390978, 0.04211898652965405387, 0.04357136537550419103, 0.04647612306720447228 ),
 ( 0.000000000000000000, 1.000000000000000000 ),
 .UNSPECIFIED. ) 
 GEOMETRIC_REPRESENTATION_ITEM ( )  RATIONAL_B_SPLINE_SURFACE ( (
 ( 1.000000000000000000, 0.6290213284793357840, 1.000000000000000000),
 ( 1.000000000000000000, 0.6248939334218988062, 1.000000000000000000),
 ( 1.000000000000000000, 0.6231525367052294095, 1.000000000000000000),
 ( 1.000000000000000000, 0.6225790212148355485, 1.000000000000000000),
 ( 1.000000000000000000, 0.6227321005834843826, 1.000000000000000000),
 ( 1.000000000000000000, 0.6234255931488940083, 1.000000000000000000),
 ( 1.000000000000000000, 0.6239617638513688114, 1.000000000000000000),
 ( 1.000000000000000000, 0.6251439415237010078, 1.000000000000000000),
 ( 1.000000000000000000, 0.6257917911431671865, 1.000000000000000000),
 ( 1.000000000000000000, 0.6269741839755182955, 1.000000000000000000),
 ( 1.000000000000000000, 0.6274966600224924917, 1.000000000000000000),
 ( 1.000000000000000000, 0.6282667852389482999, 1.000000000000000000),
 ( 1.000000000000000000, 0.6285148503998102543, 1.000000000000000000),
 ( 1.000000000000000000, 0.6286307432047592014, 1.000000000000000000),
 ( 1.000000000000000000, 0.6286269973787815823, 1.000000000000000000),
 ( 1.000000000000000000, 0.6285335994519584135, 1.000000000000000000),
 ( 1.000000000000000000, 0.6284444584874891992, 1.000000000000000000),
 ( 1.000000000000000000, 0.6280613430741410763, 1.000000000000000000),
 ( 1.000000000000000000, 0.6276496514169409568, 1.000000000000000000),
 ( 1.000000000000000000, 0.6268798492406927325, 1.000000000000000000),
 ( 1.000000000000000000, 0.6265983628749475232, 1.000000000000000000),
 ( 1.000000000000000000, 0.6260058463378762594, 1.000000000000000000),
 ( 1.000000000000000000, 0.6256937179550182693, 1.000000000000000000),
 ( 1.000000000000000000, 0.6241358698957584217, 1.000000000000000000),
 ( 1.000000000000000000, 0.6228888902089158019, 1.000000000000000000),
 ( 1.000000000000000000, 0.6226627606244575786, 1.000000000000000000),
 ( 1.000000000000000000, 0.6226866229701797373, 1.000000000000000000),
 ( 1.000000000000000000, 0.6229108014427007234, 1.000000000000000000),
 ( 1.000000000000000000, 0.6231102808943920213, 1.000000000000000000),
 ( 1.000000000000000000, 0.6240167787603944083, 1.000000000000000000),
 ( 1.000000000000000000, 0.6250322308941094196, 1.000000000000000000),
 ( 1.000000000000000000, 0.6273487183751635943, 1.000000000000000000),
 ( 1.000000000000000000, 0.6282530044593329643, 1.000000000000000000),
 ( 1.000000000000000000, 0.6303541273114475763, 1.000000000000000000),
 ( 1.000000000000000000, 0.6315549423244221083, 1.000000000000000000),
 ( 1.000000000000000000, 0.6356032421436564883, 1.000000000000000000),
 ( 1.000000000000000000, 0.6388921020275880602, 1.000000000000000000),
 ( 1.000000000000000000, 0.6428092274089116653, 1.000000000000000000) ) ) 
 REPRESENTATION_ITEM ( '' )  SURFACE ( )  );
#2700 = ORIENTED_EDGE ( 'NONE', *, *, #9245, .T. ) ;
#2701 = CARTESIAN_POINT ( 'NONE',  ( -30.13956425491234725, -21.05198877411829272, -2.800654218530471251 ) ) ;
#2702 = CARTESIAN_POINT ( 'NONE',  ( -2.999999999999998668, 22.00000000000000355, 8.485281374238567764 ) ) ;
#2703 = VERTEX_POINT ( 'NONE', #11843 ) ;
#2704 = CARTESIAN_POINT ( 'NONE',  ( -3.000000000000000000, 16.00000000000000000, 8.485281374238567764 ) ) ;
#2705 = EDGE_CURVE ( 'NONE', #12156, #5124, #17853, .T. ) ;
#2706 = CIRCLE ( 'NONE', #22101, 11.00000000000003730 ) ;
#2707 = ORIENTED_EDGE ( 'NONE', *, *, #21736, .F. ) ;
#2708 = CARTESIAN_POINT ( 'NONE',  ( -13.74639653023205277, 28.96193690644924246, -7.000000000000006217 ) ) ;
#2709 = CONICAL_SURFACE ( 'NONE', #10364, 2.099999999999997868, 1.029744258676653867 ) ;
#2710 = DIRECTION ( 'NONE',  ( 0.000000000000000000, 1.000000000000000000, 0.000000000000000000 ) ) ;
#2711 = FACE_OUTER_BOUND ( 'NONE', #8187, .T. ) ;
#2712 = DIRECTION ( 'NONE',  ( 0.000000000000000000, 1.000000000000000000, -0.000000000000000000 ) ) ;
#2713 = AXIS2_PLACEMENT_3D ( 'NONE', #11467, #8146, #6425 ) ;
#2714 = AXIS2_PLACEMENT_3D ( 'NONE', #1442, #8428, #15056 ) ;
#2715 = CARTESIAN_POINT ( 'NONE',  ( 14.30873905802343415, 28.06260833510304664, -6.999999999999950262 ) ) ;
#2716 = EDGE_CURVE ( 'NONE', #20782, #12370, #2143, .T. ) ;
#2717 = CARTESIAN_POINT ( 'NONE',  ( 3.330669073875469621E-13, -1.110223024625156540E-13, -2.999999999999971578 ) ) ;
#2718 = VERTEX_POINT ( 'NONE', #16895 ) ;
#2719 = EDGE_LOOP ( 'NONE', ( #4492, #6449, #8085, #81 ) ) ;
#2720 = EDGE_CURVE ( 'NONE', #13383, #15997, #1777, .T. ) ;
#2721 = COLOUR_RGB ( '',0.7921568627450980005, 0.8196078431372548767, 0.9333333333333333481 ) ;
#2722 = VERTEX_POINT ( 'NONE', #9569 ) ;
#2723 = CARTESIAN_POINT ( 'NONE',  ( -16.50118549063250484, 8.665255721999203686, 59.66909312737204374 ) ) ;
#2724 = DIRECTION ( 'NONE',  ( -6.505213034913038160E-19, -3.903127820947822896E-18, -1.000000000000000000 ) ) ;
#2725 = CARTESIAN_POINT ( 'NONE',  ( -2.498922976470538515, 0.1467742037829277146, -52.32005940076825112 ) ) ;
#2726 = LINE ( 'NONE', #17958, #7374 ) ;
#2727 = AXIS2_PLACEMENT_3D ( 'NONE', #16544, #19769, #846 ) ;
#2728 = FACE_OUTER_BOUND ( 'NONE', #6014, .T. ) ;
#2729 = CARTESIAN_POINT ( 'NONE',  ( 2.546974693918149679, 39.84782899243125343, 51.61921092574152681 ) ) ;
#2730 = FACE_OUTER_BOUND ( 'NONE', #8226, .T. ) ;
#2731 = CARTESIAN_POINT ( 'NONE',  ( -2.576224933361803249, 39.84426458497839718, -51.65025110505525419 ) ) ;
#2732 = DIRECTION ( 'NONE',  ( 2.659909329831104080E-15, 0.000000000000000000, 1.000000000000000000 ) ) ;
#2733 = ORIENTED_EDGE ( 'NONE', *, *, #21057, .T. ) ;
#2734 = CARTESIAN_POINT ( 'NONE',  ( 35.00000000000000000, 13.99999999999999822, -14.99999999999997691 ) ) ;
#2735 = DIRECTION ( 'NONE',  ( 1.000000000000000000, 0.000000000000000000, 0.000000000000000000 ) ) ;
#2736 = FACE_OUTER_BOUND ( 'NONE', #2926, .T. ) ;
#2737 = DIRECTION ( 'NONE',  ( 0.000000000000000000, 1.000000000000000000, 0.000000000000000000 ) ) ;
#2738 = ORIENTED_EDGE ( 'NONE', *, *, #7323, .F. ) ;
#2739 = CARTESIAN_POINT ( 'NONE',  ( -33.99999999999998579, 8.251288694035750382, 0.000000000000000000 ) ) ;
#2740 = CARTESIAN_POINT ( 'NONE',  ( 34.65667543218833657, 4.170748987303380062, 2.999999999999999112 ) ) ;
#2741 = EDGE_CURVE ( 'NONE', #10740, #2718, #7858, .T. ) ;
#2742 = CARTESIAN_POINT ( 'NONE',  ( -3.235223465815032728, -4.647308930658605952, -47.76313845446086503 ) ) ;
#2743 = DIRECTION ( 'NONE',  ( -0.000000000000000000, -1.000000000000000000, -0.000000000000000000 ) ) ;
#2744 = EDGE_CURVE ( 'NONE', #10749, #11797, #2126, .T. ) ;
#2745 = EDGE_CURVE ( 'NONE', #8634, #14562, #13436, .T. ) ;
#2746 = AXIS2_PLACEMENT_3D ( 'NONE', #6857, #22684, #20946 ) ;
#2747 = CARTESIAN_POINT ( 'NONE',  ( -4.359932693009644117E-14, -1.500000000000015987, 19.99999999999999289 ) ) ;
#2748 = CARTESIAN_POINT ( 'NONE',  ( -42.50000000000000711, -12.00000000000000000, -47.50000000000000000 ) ) ;
#2749 = EDGE_LOOP ( 'NONE', ( #21722, #17724, #10308, #18794 ) ) ;
#2750 = CARTESIAN_POINT ( 'NONE',  ( 0.4976208372498681087, 39.99853765106635706, -49.11738758647563685 ) ) ;
#2751 = CARTESIAN_POINT ( 'NONE',  ( 27.84804035626045504, -24.75236754129161909, -7.000000000000006217 ) ) ;
#2752 = EDGE_CURVE ( 'NONE', #9113, #8849, #1025, .T. ) ;
#2753 = CARTESIAN_POINT ( 'NONE',  ( 2.775557561562891351E-14, 2.775557561562891351E-14, 5.750000000000001776 ) ) ;
#2754 = CARTESIAN_POINT ( 'NONE',  ( -4.925981507846746155, 40.00000000000000711, 51.57279734433891605 ) ) ;
#2755 = CIRCLE ( 'NONE', #14437, 19.11328065563152379 ) ;
#2756 = DIRECTION ( 'NONE',  ( -0.000000000000000000, -1.000000000000000000, -0.000000000000000000 ) ) ;
#2757 = CARTESIAN_POINT ( 'NONE',  ( -4.995686258823919701, 39.84470010994202482, 52.21048258191389380 ) ) ;
#2758 = CIRCLE ( 'NONE', #14439, 36.76383501243555685 ) ;
#2759 = DIRECTION ( 'NONE',  ( -1.000000000000000000, -1.208970125616044077E-17, 0.000000000000000000 ) ) ;
#2760 = ORIENTED_EDGE ( 'NONE', *, *, #20514, .T. ) ;
#2761 = CARTESIAN_POINT ( 'NONE',  ( -21.65063509461084834, 12.49999999999967848, -2.999999999999988898 ) ) ;
#2762 = DIRECTION ( 'NONE',  ( 6.505213034913038160E-19, 3.903127820947822896E-18, 1.000000000000000000 ) ) ;
#2763 = SURFACE_STYLE_FILL_AREA ( #21593 ) ;
#2764 = CARTESIAN_POINT ( 'NONE',  ( 3.608224830031758756E-13, -25.00000000000021672, -2.999999999999999112 ) ) ;
#2765 = CARTESIAN_POINT ( 'NONE',  ( 13.00000000000024336, -2.516660498395250745, 60.00099999999999767 ) ) ;
#2766 = CIRCLE ( 'NONE', #21789, 19.11328065563152379 ) ;
#2767 = ORIENTED_EDGE ( 'NONE', *, *, #22107, .F. ) ;
#2768 = CARTESIAN_POINT ( 'NONE',  ( 35.00000000000000000, -9.000000000000001776, 4.258610482196280173E-15 ) ) ;
#2769 = CARTESIAN_POINT ( 'NONE',  ( -21.94460005644892675, -28.73837443790567647, -2.932164912090524655 ) ) ;
#2770 = ORIENTED_EDGE ( 'NONE', *, *, #423, .F. ) ;
#2771 = CIRCLE ( 'NONE', #3518, 2.099999999999997868 ) ;
#2772 = VERTEX_POINT ( 'NONE', #6931 ) ;
#2773 = ADVANCED_FACE ( 'NONE', ( #8859, #3494, #18962, #11960, #141, #13987, #15829, #6812 ), #13777, .F. ) ;
#2774 = ORIENTED_EDGE ( 'NONE', *, *, #8336, .T. ) ;
#2775 = CARTESIAN_POINT ( 'NONE',  ( 17.21151300967877162, 30.19805602791846511, -59.88250013944306716 ) ) ;
#2776 = VECTOR ( 'NONE', #1461, 1000.000000000000000 ) ;
#2777 = DIRECTION ( 'NONE',  ( 0.000000000000000000, -1.000000000000000000, 0.000000000000000000 ) ) ;
#2778 = DIRECTION ( 'NONE',  ( -6.505213034913038160E-19, -3.903127820947822896E-18, -1.000000000000000000 ) ) ;
#2779 = EDGE_CURVE ( 'NONE', #7020, #20079, #10452, .T. ) ;
#2780 = DIRECTION ( 'NONE',  ( -1.445602896647339410E-16, 0.000000000000000000, -1.000000000000000000 ) ) ;
#2781 = CARTESIAN_POINT ( 'NONE',  ( 2.775557561562891351E-14, 2.775557561562891351E-14, 5.750000000000001776 ) ) ;
#2782 = ORIENTED_EDGE ( 'NONE', *, *, #14527, .F. ) ;
#2783 = FACE_OUTER_BOUND ( 'NONE', #16329, .T. ) ;
#2784 = CARTESIAN_POINT ( 'NONE',  ( 2.220446049250313081E-13, -2.498001805406602216E-13, -6.859353255829918616 ) ) ;
#2785 = VERTEX_POINT ( 'NONE', #20907 ) ;
#2786 = CARTESIAN_POINT ( 'NONE',  ( -12.06668108811420836, 11.08190912999967459, -44.43106897542661216 ) ) ;
#2787 = CARTESIAN_POINT ( 'NONE',  ( -32.89708536800386440, -15.00428685838208587, 2.932460736555834835 ) ) ;
#2788 = CARTESIAN_POINT ( 'NONE',  ( 35.00000000000000000, 0.000000000000000000, 9.000000000000007105 ) ) ;
#2789 = CARTESIAN_POINT ( 'NONE',  ( 3.995109193065607744, 40.00000000000000711, 51.09401218757847118 ) ) ;
#2790 = EDGE_LOOP ( 'NONE', ( #508, #9529 ) ) ;
#2791 = DIRECTION ( 'NONE',  ( 6.505213034913038160E-19, 3.903127820947822896E-18, 1.000000000000000000 ) ) ;
#2792 = LINE ( 'NONE', #4512, #19358 ) ;
#2793 = ADVANCED_FACE ( 'NONE', ( #8416 ), #15289, .T. ) ;
#2794 = ORIENTED_EDGE ( 'NONE', *, *, #5649, .F. ) ;
#2795 = DIRECTION ( 'NONE',  ( -0.000000000000000000, 1.000000000000000000, -0.000000000000000000 ) ) ;
#2796 = CARTESIAN_POINT ( 'NONE',  ( -6.041077103370461110, -0.8288449397156272269, 52.13906252460642321 ) ) ;
#2797 = AXIS2_PLACEMENT_3D ( 'NONE', #1781, #5537, #15958 ) ;
#2798 = VECTOR ( 'NONE', #7146, 1000.000000000000000 ) ;
#2799 = ORIENTED_EDGE ( 'NONE', *, *, #14942, .F. ) ;
#2800 = PRODUCT_DEFINITION_CONTEXT ( 'detailed design', #13389, 'design' ) ;
#2801 = DIRECTION ( 'NONE',  ( -6.505213034913038160E-19, -3.903127820947822896E-18, -1.000000000000000000 ) ) ;
#2802 = DIRECTION ( 'NONE',  ( -0.000000000000000000, 1.000000000000000000, -0.000000000000000000 ) ) ;
#2803 = AXIS2_PLACEMENT_3D ( 'NONE', #18547, #21883, #16594 ) ;
#2804 = CARTESIAN_POINT ( 'NONE',  ( 16.86148599981780194, 30.79460519221557391, -57.23208912996602749 ) ) ;
#2805 = EDGE_LOOP ( 'NONE', ( #5274, #9508, #9161, #20402 ) ) ;
#2806 = ORIENTED_EDGE ( 'NONE', *, *, #7077, .F. ) ;
#2807 = ORIENTED_EDGE ( 'NONE', *, *, #1340, .T. ) ;
#2808 = AXIS2_PLACEMENT_3D ( 'NONE', #17710, #17602, #22675 ) ;
#2809 = AXIS2_PLACEMENT_3D ( 'NONE', #2915, #5082, #18823 ) ;
#2810 = EDGE_LOOP ( 'NONE', ( #18690, #10329 ) ) ;
#2811 = CARTESIAN_POINT ( 'NONE',  ( 24.41514043009218682, 26.50842683089740959, -6.999999999999999112 ) ) ;
#2812 = ORIENTED_EDGE ( 'NONE', *, *, #21989, .F. ) ;
#2813 = CARTESIAN_POINT ( 'NONE',  ( -29.33526866242079478, 22.15900668633771886, 2.800654218530485018 ) ) ;
#2814 = CARTESIAN_POINT ( 'NONE',  ( -9.377138775076145905, -4.928932188134508507, 51.00555535510815730 ) ) ;
#2815 = ORIENTED_EDGE ( 'NONE', *, *, #3808, .F. ) ;
#2816 = CARTESIAN_POINT ( 'NONE',  ( 1.568459684869332627, 13.32608676514834301, 8.880481854261958574 ) ) ;
#2817 = AXIS2_PLACEMENT_3D ( 'NONE', #21733, #2218, #12410 ) ;
#2818 = DIRECTION ( 'NONE',  ( 0.000000000000000000, 1.000000000000000000, -0.000000000000000000 ) ) ;
#2819 = EDGE_LOOP ( 'NONE', ( #9502, #16436, #14820, #21310 ) ) ;
#2820 = CARTESIAN_POINT ( 'NONE',  ( 2.775557561562891351E-14, -2.775557561562891351E-14, 2.999999999999999112 ) ) ;
#2821 = DIRECTION ( 'NONE',  ( 1.296372316667914327E-16, 1.000000000000000000, -0.000000000000000000 ) ) ;
#2822 = DIRECTION ( 'NONE',  ( -0.000000000000000000, -1.000000000000000000, -0.000000000000000000 ) ) ;
#2823 = CARTESIAN_POINT ( 'NONE',  ( -34.65667543218827262, -4.170748987303407596, -2.999999999999971578 ) ) ;
#2824 = AXIS2_PLACEMENT_3D ( 'NONE', #2761, #6303, #9743 ) ;
#2825 = EDGE_CURVE ( 'NONE', #790, #11530, #5209, .T. ) ;
#2826 = CARTESIAN_POINT ( 'NONE',  ( -6.426802710256907858, 6.431242889908570071, 41.03786381671503847 ) ) ;
#2827 = ORIENTED_EDGE ( 'NONE', *, *, #14634, .T. ) ;
#2828 = ADVANCED_FACE ( 'NONE', ( #14104 ), #5427, .T. ) ;
#2829 = EDGE_CURVE ( 'NONE', #18519, #22196, #7986, .T. ) ;
#2830 = ORIENTED_EDGE ( 'NONE', *, *, #10117, .T. ) ;
#2831 = ORIENTED_EDGE ( 'NONE', *, *, #18843, .T. ) ;
#2832 = CARTESIAN_POINT ( 'NONE',  ( -16.86148599981783036, 30.79460519221558457, 57.23208912996606301 ) ) ;
#2833 = LINE ( 'NONE', #13339, #2309 ) ;
#2834 = B_SPLINE_CURVE_WITH_KNOTS ( 'NONE', 3,
 ( #909, #4362, #689, #7673 ),
 .UNSPECIFIED., .F., .F.,
 ( 4, 4 ),
 ( 9.545285769850769053E-07, 0.001900595205834759759 ),
 .UNSPECIFIED. ) ;
#2835 = AXIS2_PLACEMENT_3D ( 'NONE', #12849, #13071, #3011 ) ;
#2836 = DIRECTION ( 'NONE',  ( -0.000000000000000000, 1.000000000000000000, -0.000000000000000000 ) ) ;
#2837 = CARTESIAN_POINT ( 'NONE',  ( 35.00000000000000000, 0.000000000000000000, 4.258610482196280173E-15 ) ) ;
#2838 = DIRECTION ( 'NONE',  ( -6.505213034913038160E-19, -3.903127820947822896E-18, -1.000000000000000000 ) ) ;
#2839 = EDGE_CURVE ( 'NONE', #12042, #15630, #21166, .T. ) ;
#2840 = VERTEX_POINT ( 'NONE', #20675 ) ;
#2841 = DIRECTION ( 'NONE',  ( 6.505213034913038160E-19, 3.903127820947822896E-18, 1.000000000000000000 ) ) ;
#2842 = LINE ( 'NONE', #21867, #10831 ) ;
#2843 = CARTESIAN_POINT ( 'NONE',  ( -27.64365646977254443, -17.09029715894946833, 3.000000000000012879 ) ) ;
#2844 = CARTESIAN_POINT ( 'NONE',  ( -7.464612179280154969, 38.57206774498447288, -54.30634996223604105 ) ) ;
#2845 = DIRECTION ( 'NONE',  ( -0.000000000000000000, 1.000000000000000000, -0.000000000000000000 ) ) ;
#2846 = EDGE_LOOP ( 'NONE', ( #15417, #10007, #14803, #8317 ) ) ;
#2847 = AXIS2_PLACEMENT_3D ( 'NONE', #3112, #11479, #18699 ) ;
#2848 = TOROIDAL_SURFACE ( 'NONE', #1754, 34.90673715956759082, 8.750000000000000000 ) ;
#2849 = CARTESIAN_POINT ( 'NONE',  ( 42.50000000000000711, -11.97499999999999964, 47.50000000000000711 ) ) ;
#2850 = DIRECTION ( 'NONE',  ( 6.505213034913038160E-19, 3.903127820947822896E-18, 1.000000000000000000 ) ) ;
#2851 = CARTESIAN_POINT ( 'NONE',  ( 35.00000000000000000, 40.00000000000000000, 4.258610482196280173E-15 ) ) ;
#2852 = EDGE_CURVE ( 'NONE', #11430, #14282, #3269, .T. ) ;
#2853 = DIRECTION ( 'NONE',  ( -1.000000000000000000, 0.000000000000000000, 0.000000000000000000 ) ) ;
#2854 = ORIENTED_EDGE ( 'NONE', *, *, #2779, .T. ) ;
#2855 = AXIS2_PLACEMENT_3D ( 'NONE', #4502, #20089, #13181 ) ;
#2856 = CARTESIAN_POINT ( 'NONE',  ( 31.11077005834453502, -4.936596639065232495, 2.999999999999995559 ) ) ;
#2857 = CARTESIAN_POINT ( 'NONE',  ( -0.7809641287214766914, -4.625293788890096458, -46.06432795380058565 ) ) ;
#2858 = AXIS2_PLACEMENT_3D ( 'NONE', #7912, #21898, #7789 ) ;
#2859 = CARTESIAN_POINT ( 'NONE',  ( 27.56232195404084706, -21.41958700883264655, -2.999999999999954259 ) ) ;
#2860 = VECTOR ( 'NONE', #86, 1000.000000000000000 ) ;
#2861 = EDGE_CURVE ( 'NONE', #14184, #1555, #463, .T. ) ;
#2862 = CARTESIAN_POINT ( 'NONE',  ( 1.564866216807978994, -1.162741450739184890, 47.08240428779123476 ) ) ;
#2863 = VECTOR ( 'NONE', #17832, 1000.000000000000114 ) ;
#2864 = CARTESIAN_POINT ( 'NONE',  ( -42.50000000000000711, -11.97499999999999964, -47.50000000000000000 ) ) ;
#2865 = ORIENTED_EDGE ( 'NONE', *, *, #3, .F. ) ;
#2866 = VECTOR ( 'NONE', #10233, 1000.000000000000000 ) ;
#2867 = DIRECTION ( 'NONE',  ( 1.734723475976892686E-15, 0.000000000000000000, 1.000000000000000000 ) ) ;
#2868 = EDGE_CURVE ( 'NONE', #12296, #7531, #10896, .T. ) ;
#2869 = DIRECTION ( 'NONE',  ( -0.000000000000000000, -1.000000000000000000, -0.000000000000000000 ) ) ;
#2870 = CARTESIAN_POINT ( 'NONE',  ( -5.188160884119104033, 39.99999999999999289, 51.70385028745301526 ) ) ;
#2871 = DIRECTION ( 'NONE',  ( 1.296372316667914327E-16, 1.000000000000000000, -0.000000000000000000 ) ) ;
#2872 = AXIS2_PLACEMENT_3D ( 'NONE', #2901, #4499, #18590 ) ;
#2873 = CARTESIAN_POINT ( 'NONE',  ( -10.38193264731105003, 30.83255023748042944, -43.52061562521058136 ) ) ;
#2874 = LINE ( 'NONE', #4710, #2262 ) ;
#2875 = VERTEX_POINT ( 'NONE', #15498 ) ;
#2876 = CARTESIAN_POINT ( 'NONE',  ( 14.52224280010135793, 23.83254695043585514, 45.61498238574513664 ) ) ;
#2877 = CARTESIAN_POINT ( 'NONE',  ( 1.110223024625156540E-13, -5.551115123125782702E-14, -6.999999999999950262 ) ) ;
#2878 = DIRECTION ( 'NONE',  ( 1.296372316667914327E-16, 1.000000000000000000, -0.000000000000000000 ) ) ;
#2879 = ADVANCED_FACE ( 'NONE', ( #22518 ), #19072, .F. ) ;
#2880 = EDGE_CURVE ( 'NONE', #11090, #16909, #17127, .T. ) ;
#2881 = CARTESIAN_POINT ( 'NONE',  ( -0.005835298841899191902, 39.99999999999999289, -48.73851474269406481 ) ) ;
#2882 = VERTEX_POINT ( 'NONE', #1656 ) ;
#2883 =( REPRESENTATION_RELATIONSHIP ('NONE','NONE', #8442, #13507 ) REPRESENTATION_RELATIONSHIP_WITH_TRANSFORMATION ( #222 )SHAPE_REPRESENTATION_RELATIONSHIP( ) );
#2884 = VECTOR ( 'NONE', #11383, 1000.000000000000000 ) ;
#2885 = CARTESIAN_POINT ( 'NONE',  ( -1.387778780781445676E-14, 20.00000000000000000, -101.0000000000000284 ) ) ;
#2886 = CARTESIAN_POINT ( 'NONE',  ( 34.65667543218853552, 4.170748987303296573, -2.999999999999975131 ) ) ;
#2887 = CIRCLE ( 'NONE', #3984, 22.12933039895921539 ) ;
#2888 = VECTOR ( 'NONE', #11317, 1000.000000000000000 ) ;
#2889 = EDGE_CURVE ( 'NONE', #5874, #11652, #16575, .T. ) ;
#2890 = AXIS2_PLACEMENT_3D ( 'NONE', #7003, #6777, #13959 ) ;
#2891 = EDGE_LOOP ( 'NONE', ( #17547, #17921, #11604, #5644 ) ) ;
#2892 = EDGE_LOOP ( 'NONE', ( #1882, #5395 ) ) ;
#2893 = EDGE_CURVE ( 'NONE', #10333, #10996, #14180, .T. ) ;
#2894 = ORIENTED_EDGE ( 'NONE', *, *, #15318, .T. ) ;
#2895 = CARTESIAN_POINT ( 'NONE',  ( 10.95224849132198131, 40.00000000000000000, 53.95427542910576335 ) ) ;
#2896 = DIRECTION ( 'NONE',  ( -0.000000000000000000, -1.000000000000000000, -0.000000000000000000 ) ) ;
#2897 = PLANE ( 'NONE',  #16863 ) ;
#2898 = CARTESIAN_POINT ( 'NONE',  ( 18.99836266309356247, 13.69920652258249483, 60.37582729383724001 ) ) ;
#2899 = EDGE_CURVE ( 'NONE', #1869, #7355, #7256, .T. ) ;
#2900 =( GEOMETRIC_REPRESENTATION_CONTEXT ( 3 ) GLOBAL_UNCERTAINTY_ASSIGNED_CONTEXT ( ( #11243 ) ) GLOBAL_UNIT_ASSIGNED_CONTEXT ( ( #17257, #8792, #12436 ) ) REPRESENTATION_CONTEXT ( 'NONE', 'WORKASPACE' ) );
#2901 = CARTESIAN_POINT ( 'NONE',  ( 35.00000000000000000, 0.000000000000000000, 4.258610482196280173E-15 ) ) ;
#2902 = VERTEX_POINT ( 'NONE', #7593 ) ;
#2903 = FACE_OUTER_BOUND ( 'NONE', #3500, .T. ) ;
#2905 = CONICAL_SURFACE ( 'NONE', #13466, 2.525000000000110489, 0.7853981633971014453 ) ;
#2904 = CARTESIAN_POINT ( 'NONE',  ( -15.00000000000001421, 20.00000000000000000, -101.0000000000000284 ) ) ;
#2906 = ORIENTED_EDGE ( 'NONE', *, *, #3732, .T. ) ;
#2907 = CARTESIAN_POINT ( 'NONE',  ( -35.00000000000058265, 26.00000000000000355, -57.10000000000076170 ) ) ;
#2908 = DIRECTION ( 'NONE',  ( 0.000000000000000000, 1.000000000000000000, 0.000000000000000000 ) ) ;
#2909 = DIRECTION ( 'NONE',  ( 0.000000000000000000, 1.000000000000000000, 0.000000000000000000 ) ) ;
#2910 = CARTESIAN_POINT ( 'NONE',  ( 2.774848782070428399, 40.00000000000000000, 50.42374031262293954 ) ) ;
#2911 = ORIENTED_EDGE ( 'NONE', *, *, #5631, .F. ) ;
#2912 = CARTESIAN_POINT ( 'NONE',  ( -15.12081897056648216, 33.51030287062351221, -1.999999999999977573 ) ) ;
#2913 = DIRECTION ( 'NONE',  ( -0.000000000000000000, -1.000000000000000000, -0.000000000000000000 ) ) ;
#2914 = ORIENTED_EDGE ( 'NONE', *, *, #20129, .F. ) ;
#2915 = CARTESIAN_POINT ( 'NONE',  ( -7.094908322883064500, 35.33352588067081967, 3.000000000000023537 ) ) ;
#2916 = AXIS2_PLACEMENT_3D ( 'NONE', #12951, #16629, #2438 ) ;
#2917 = CARTESIAN_POINT ( 'NONE',  ( 2.432942025170123296E-14, -0.5379598322809753252, -48.80682109170825100 ) ) ;
#2918 = ORIENTED_EDGE ( 'NONE', *, *, #20893, .T. ) ;
#2919 = CARTESIAN_POINT ( 'NONE',  ( -4.171001175319322130, -35.79662727779903264, 3.000000000000023537 ) ) ;
#2920 = CARTESIAN_POINT ( 'NONE',  ( 2.775557561562891351E-13, 3.000000000000002665, -5.000000000000004441 ) ) ;
#2921 = CARTESIAN_POINT ( 'NONE',  ( 35.00000000000058265, 40.00000000000000000, -55.00000000000076028 ) ) ;
#2922 = ADVANCED_FACE ( 'NONE', ( #14449 ), #16770, .T. ) ;
#2923 = CARTESIAN_POINT ( 'NONE',  ( 16.50118549063284590, 8.665255721999795213, -59.66909312737200821 ) ) ;
#2924 = AXIS2_PLACEMENT_3D ( 'NONE', #12514, #12753, #3836 ) ;
#2925 = ORIENTED_EDGE ( 'NONE', *, *, #20473, .F. ) ;
#2926 = EDGE_LOOP ( 'NONE', ( #18294, #17238, #3471, #14348, #5498, #3287 ) ) ;
#2927 = EDGE_CURVE ( 'NONE', #2593, #18617, #2447, .T. ) ;
#2928 = ORIENTED_EDGE ( 'NONE', *, *, #5415, .T. ) ;
#2929 = EDGE_LOOP ( 'NONE', ( #22524, #13285 ) ) ;
#2930 = CARTESIAN_POINT ( 'NONE',  ( 2.615521992591937295, 23.51527106174855675, 6.613019222498396132 ) ) ;
#2931 = VERTEX_POINT ( 'NONE', #4163 ) ;
#2932 = DIRECTION ( 'NONE',  ( 6.505213034913038160E-19, 3.903127820947822896E-18, 1.000000000000000000 ) ) ;
#2933 = CARTESIAN_POINT ( 'NONE',  ( -5.770190843045729601, -4.767707482271699604, -49.21533144469186283 ) ) ;
#2934 = ORIENTED_EDGE ( 'NONE', *, *, #20496, .F. ) ;
#2935 = CARTESIAN_POINT ( 'NONE',  ( 3.000000000000000888, 15.99999999999999645, 6.485281374238567764 ) ) ;
#2936 = LINE ( 'NONE', #22150, #15177 ) ;
#2937 = EDGE_LOOP ( 'NONE', ( #21696, #5503, #19295, #1870 ) ) ;
#2938 = CARTESIAN_POINT ( 'NONE',  ( 4.628075497661257032, 39.46063506869912629, -53.65703709786517805 ) ) ;
#2939 = DIRECTION ( 'NONE',  ( 0.000000000000000000, -1.000000000000000000, 0.000000000000000000 ) ) ;
#2940 = CARTESIAN_POINT ( 'NONE',  ( -34.88850421923980605, 1.128083539116031542, 2.999999999999995559 ) ) ;
#2941 = CARTESIAN_POINT ( 'NONE',  ( -17.70396115872096132, 29.35428329955201576, -60.02641142872582236 ) ) ;
#2942 = EDGE_CURVE ( 'NONE', #11842, #14574, #9813, .T. ) ;
#2943 = AXIS2_PLACEMENT_3D ( 'NONE', #8132, #16377, #4128 ) ;
#2944 = CARTESIAN_POINT ( 'NONE',  ( 2.775557561562891351E-14, 2.775557561562891351E-14, 5.750000000000001776 ) ) ;
#2945 = VERTEX_POINT ( 'NONE', #19754 ) ;
#2946 = ORIENTED_EDGE ( 'NONE', *, *, #645, .T. ) ;
#2947 = AXIS2_PLACEMENT_3D ( 'NONE', #10906, #18348, #7477 ) ;
#2948 = EDGE_CURVE ( 'NONE', #4189, #2718, #12723, .T. ) ;
#2949 = VERTEX_POINT ( 'NONE', #18132 ) ;
#2950 = CARTESIAN_POINT ( 'NONE',  ( -19.64963058618614511, 23.83053889022995619, 60.53829769526753779 ) ) ;
#2951 = DIRECTION ( 'NONE',  ( 1.000000000000000000, 1.208970125616067650E-17, 0.000000000000000000 ) ) ;
#2952 = CARTESIAN_POINT ( 'NONE',  ( -16.30820259622267088, 8.415540886845235491, -59.60694662124532073 ) ) ;
#2953 = CARTESIAN_POINT ( 'NONE',  ( 12.99999999999993960, 42.51666049839543149, -105.0000000000000142 ) ) ;
#2954 = EDGE_CURVE ( 'NONE', #17558, #7013, #4701, .T. ) ;
#2955 = AXIS2_PLACEMENT_3D ( 'NONE', #8908, #19572, #19462 ) ;
#2956 = PLANE ( 'NONE',  #21445 ) ;
#2957 = VERTEX_POINT ( 'NONE', #16411 ) ;
#2958 = CYLINDRICAL_SURFACE ( 'NONE', #20451, 2.099999999999997868 ) ;
#2959 = CARTESIAN_POINT ( 'NONE',  ( -0.9873823818543894237, 39.99999999999998579, -49.36449638065314360 ) ) ;
#2960 = CARTESIAN_POINT ( 'NONE',  ( 36.54278193890331039, 4.025500340002458266, 2.800654218530485018 ) ) ;
#2961 = LINE ( 'NONE', #7881, #22187 ) ;
#2962 = EDGE_CURVE ( 'NONE', #7988, #14674, #7621, .T. ) ;
#2963 = ORIENTED_EDGE ( 'NONE', *, *, #3662, .T. ) ;
#2964 = CARTESIAN_POINT ( 'NONE',  ( 28.07080038625092655, 14.29266125237893448, -2.999999999999999112 ) ) ;
#2965 = DIRECTION ( 'NONE',  ( -0.000000000000000000, -1.000000000000000000, -0.000000000000000000 ) ) ;
#2966 = VERTEX_POINT ( 'NONE', #483 ) ;
#2967 = DIRECTION ( 'NONE',  ( 0.000000000000000000, 0.000000000000000000, 1.000000000000000000 ) ) ;
#2968 = CARTESIAN_POINT ( 'NONE',  ( -34.65667543218827262, -4.170748987303407596, -2.999999999999971578 ) ) ;
#2969 = DIRECTION ( 'NONE',  ( 0.000000000000000000, 0.000000000000000000, 1.000000000000000000 ) ) ;
#2970 = CARTESIAN_POINT ( 'NONE',  ( -25.00000000000000000, 20.00000000000000000, -25.00000000000000000 ) ) ;
#2971 = CIRCLE ( 'NONE', #15753, 36.76383501243555685 ) ;
#2972 = ORIENTED_EDGE ( 'NONE', *, *, #3652, .F. ) ;
#2973 = CIRCLE ( 'NONE', #7343, 1.000000000000000888 ) ;
#2974 = ORIENTED_EDGE ( 'NONE', *, *, #2433, .T. ) ;
#2975 = DIRECTION ( 'NONE',  ( -1.000000000000000000, 0.000000000000000000, 0.000000000000000000 ) ) ;
#2976 = CYLINDRICAL_SURFACE ( 'NONE', #7979, 2.499999999999996891 ) ;
#2977 = ORIENTED_EDGE ( 'NONE', *, *, #5631, .T. ) ;
#2978 = CARTESIAN_POINT ( 'NONE',  ( 8.256135806678233990, -0.3920627093407412778, 55.63523492903830459 ) ) ;
#2979 = AXIS2_PLACEMENT_3D ( 'NONE', #21518, #4894, #5011 ) ;
#2980 = CARTESIAN_POINT ( 'NONE',  ( 42.50000000000000711, -12.00000000000000000, 47.50000000000000711 ) ) ;
#2981 = CARTESIAN_POINT ( 'NONE',  ( -9.952189117650851458, 40.00000000000000000, -53.64426396172072486 ) ) ;
#2982 = DIRECTION ( 'NONE',  ( -0.000000000000000000, -0.000000000000000000, 1.000000000000000000 ) ) ;
#2983 = CARTESIAN_POINT ( 'NONE',  ( -14.40375226887236515, 24.20453657423045968, -45.56106839101555295 ) ) ;
#2984 = EDGE_CURVE ( 'NONE', #8022, #6315, #11312, .T. ) ;
#2985 = DIRECTION ( 'NONE',  ( -0.000000000000000000, 1.000000000000000000, -0.000000000000000000 ) ) ;
#2986 = ORIENTED_EDGE ( 'NONE', *, *, #20605, .F. ) ;
#2987 = CARTESIAN_POINT ( 'NONE',  ( 14.87996495114178508, 21.93329436794035914, 45.77322900830825603 ) ) ;
#2988 = DIRECTION ( 'NONE',  ( -1.000000000000000000, -1.208970125616014957E-17, 0.000000000000000000 ) ) ;
#2989 = DIRECTION ( 'NONE',  ( 0.000000000000000000, 0.000000000000000000, -1.000000000000000000 ) ) ;
#2990 = CARTESIAN_POINT ( 'NONE',  ( -34.99999999999998579, -3.999999999999985345, -59.99999999999703704 ) ) ;
#2991 = ORIENTED_EDGE ( 'NONE', *, *, #3871, .T. ) ;
#2992 = CARTESIAN_POINT ( 'NONE',  ( -28.96193690644939522, -14.74639653023249153, 2.999999999999995559 ) ) ;
#2993 = CARTESIAN_POINT ( 'NONE',  ( -22.15900668633755188, -29.33526866242114295, -2.800654218530433059 ) ) ;
#2994 = CIRCLE ( 'NONE', #8481, 19.11328065563151668 ) ;
#2995 = EDGE_CURVE ( 'NONE', #12838, #21713, #1441, .T. ) ;
#2996 = EDGE_LOOP ( 'NONE', ( #4896, #14681, #2460, #14741, #12315, #14007 ) ) ;
#2997 = ORIENTED_EDGE ( 'NONE', *, *, #19076, .T. ) ;
#2998 = CONTEXT_DEPENDENT_SHAPE_REPRESENTATION ( #20883, #9495 ) ;
#2999 = ADVANCED_FACE ( 'NONE', ( #21460 ), #7480, .T. ) ;
#3000 = EDGE_CURVE ( 'NONE', #13430, #14951, #3285, .T. ) ;
#3001 = ORIENTED_EDGE ( 'NONE', *, *, #3202, .F. ) ;
#3002 = CARTESIAN_POINT ( 'NONE',  ( 14.29266125237896290, -28.07080038625095497, 3.000000000000002665 ) ) ;
#3003 = CARTESIAN_POINT ( 'NONE',  ( 10.27431133777208316, -4.928932188134517389, 51.43682631505490832 ) ) ;
#3004 = CYLINDRICAL_SURFACE ( 'NONE', #16835, 9.000000000000003553 ) ;
#3005 = CARTESIAN_POINT ( 'NONE',  ( -10.01544929272295192, 34.09574698892465250, 3.000000000000057732 ) ) ;
#3006 = CARTESIAN_POINT ( 'NONE',  ( -2.114046819835667446, 5.114762345337546812, -38.90380387758576575 ) ) ;
#3007 = ORIENTED_EDGE ( 'NONE', *, *, #12807, .F. ) ;
#3008 = CARTESIAN_POINT ( 'NONE',  ( 35.00000000000000000, 38.99999999999999289, 4.258610482196280173E-15 ) ) ;
#3009 = DIRECTION ( 'NONE',  ( -0.000000000000000000, 1.000000000000000000, -0.000000000000000000 ) ) ;
#3010 = ORIENTED_EDGE ( 'NONE', *, *, #7740, .F. ) ;
#3011 = DIRECTION ( 'NONE',  ( -1.000000000000000000, -1.208970125616077665E-17, 0.000000000000000000 ) ) ;
#3012 = FACE_OUTER_BOUND ( 'NONE', #8975, .T. ) ;
#3013 = CIRCLE ( 'NONE', #18001, 6.499999999999999112 ) ;
#3014 = CARTESIAN_POINT ( 'NONE',  ( -34.99999999999999289, 4.000000000000028422, -3.012171160963566127E-14 ) ) ;
#3015 = CARTESIAN_POINT ( 'NONE',  ( 9.952189117650764416, 40.00000000000000000, 53.64426396172094513 ) ) ;
#3016 = ORIENTED_EDGE ( 'NONE', *, *, #22148, .T. ) ;
#3017 = CARTESIAN_POINT ( 'NONE',  ( -9.066530188944724955, 39.99999999999999289, -53.36211916096569752 ) ) ;
#3018 = ORIENTED_EDGE ( 'NONE', *, *, #5005, .F. ) ;
#3019 = CARTESIAN_POINT ( 'NONE',  ( -6.000000000000000888, 0.000000000000000000, -5.999999999999998224 ) ) ;
#3020 = PRESENTATION_STYLE_ASSIGNMENT (( #17685 ) ) ;
#3021 = ORIENTED_EDGE ( 'NONE', *, *, #4693, .T. ) ;
#3022 = CARTESIAN_POINT ( 'NONE',  ( 30.48934413892778750, -16.99647590252659057, 3.000000000000027089 ) ) ;
#3023 = DIRECTION ( 'NONE',  ( -0.000000000000000000, -1.000000000000000000, -0.000000000000000000 ) ) ;
#3024 = CYLINDRICAL_SURFACE ( 'NONE', #17665, 34.00000000000000000 ) ;
#3025 = CARTESIAN_POINT ( 'NONE',  ( 19.27753112431989635, 25.39788459340050153, -57.95296232962348171 ) ) ;
#3026 = EDGE_CURVE ( 'NONE', #21259, #8676, #13482, .T. ) ;
#3027 = EDGE_LOOP ( 'NONE', ( #19847, #19122, #3846, #7657 ) ) ;
#3028 = VECTOR ( 'NONE', #1480, 1000.000000000000000 ) ;
#3029 = ORIENTED_EDGE ( 'NONE', *, *, #2200, .T. ) ;
#3030 = VERTEX_POINT ( 'NONE', #12739 ) ;
#3031 = EDGE_CURVE ( 'NONE', #19508, #17065, #3824, .T. ) ;
#3032 = EDGE_CURVE ( 'NONE', #22365, #18209, #4740, .T. ) ;
#3033 = ORIENTED_EDGE ( 'NONE', *, *, #22659, .F. ) ;
#3034 = CARTESIAN_POINT ( 'NONE',  ( 10.95789470907245189, 39.14627205505679086, 55.00167764548202598 ) ) ;
#3035 = DIRECTION ( 'NONE',  ( 0.000000000000000000, 1.000000000000000000, 0.000000000000000000 ) ) ;
#3036 = DIRECTION ( 'NONE',  ( 1.000000000000000000, -0.000000000000000000, 0.000000000000000000 ) ) ;
#3037 = ORIENTED_EDGE ( 'NONE', *, *, #16349, .F. ) ;
#3038 = CARTESIAN_POINT ( 'NONE',  ( 35.00000000000000000, 40.00000000000000000, 4.258610482196280173E-15 ) ) ;
#3039 = DIRECTION ( 'NONE',  ( 0.000000000000000000, -0.7071067811865302533, -0.7071067811865647812 ) ) ;
#3040 = VERTEX_POINT ( 'NONE', #9090 ) ;
#3041 = FACE_BOUND ( 'NONE', #7156, .T. ) ;
#3042 = VERTEX_POINT ( 'NONE', #7367 ) ;
#3043 = FACE_OUTER_BOUND ( 'NONE', #10903, .T. ) ;
#3044 = EDGE_CURVE ( 'NONE', #4376, #13677, #16435, .T. ) ;
#3045 = CARTESIAN_POINT ( 'NONE',  ( -6.000000000000000888, -40.00000000000000000, -5.999999999999998224 ) ) ;
#3046 = CARTESIAN_POINT ( 'NONE',  ( 16.66666666666669272, 20.00000000000000000, -23.57022603955159212 ) ) ;
#3047 = CARTESIAN_POINT ( 'NONE',  ( -15.58352763714665556, 32.54529335663308842, -59.37339313163356991 ) ) ;
#3048 = CIRCLE ( 'NONE', #21707, 1.999999999999999778 ) ;
#3049 = CARTESIAN_POINT ( 'NONE',  ( -11.84374239103370563, 10.78799321809638734, 44.31542800769557289 ) ) ;
#3050 = EDGE_LOOP ( 'NONE', ( #11360, #15711 ) ) ;
#3051 = ORIENTED_EDGE ( 'NONE', *, *, #3059, .F. ) ;
#3052 = ORIENTED_EDGE ( 'NONE', *, *, #5972, .T. ) ;
#3053 = ORIENTED_EDGE ( 'NONE', *, *, #13561, .F. ) ;
#3054 = CARTESIAN_POINT ( 'NONE',  ( -19.88294660283940374, 17.66261523023111124, 60.59423886784515645 ) ) ;
#3055 = DIRECTION ( 'NONE',  ( -1.000000000000000000, 0.000000000000000000, 0.000000000000000000 ) ) ;
#3056 = CARTESIAN_POINT ( 'NONE',  ( -7.711478842616553919, 31.57187188083510065, 3.000000000000023537 ) ) ;
#3057 = CARTESIAN_POINT ( 'NONE',  ( -42.50000000000000711, -5.000000000000000000, 47.50000000000000711 ) ) ;
#3058 = AXIS2_PLACEMENT_3D ( 'NONE', #19171, #22502, #3132 ) ;
#3059 = EDGE_CURVE ( 'NONE', #10976, #4064, #5463, .T. ) ;
#3060 = EDGE_CURVE ( 'NONE', #11765, #11771, #13127, .T. ) ;
#3061 = DIRECTION ( 'NONE',  ( 6.505213034913038160E-19, 3.903127820947822896E-18, 1.000000000000000000 ) ) ;
#3062 = ORIENTED_EDGE ( 'NONE', *, *, #5369, .F. ) ;
#3063 = CARTESIAN_POINT ( 'NONE',  ( -35.16985127952374057, -10.70799354677395776, -2.800654218530457484 ) ) ;
#3064 = DIRECTION ( 'NONE',  ( -0.000000000000000000, 1.000000000000000000, -0.000000000000000000 ) ) ;
#3065 = CARTESIAN_POINT ( 'NONE',  ( -42.50000000000000000, 10.00000000000000000, 47.49999999999999289 ) ) ;
#3066 = AXIS2_PLACEMENT_3D ( 'NONE', #2254, #18053, #415 ) ;
#3067 = EDGE_LOOP ( 'NONE', ( #4156, #14561, #11052, #2355 ) ) ;
#3068 = EDGE_CURVE ( 'NONE', #17245, #22326, #18702, .T. ) ;
#3069 = CARTESIAN_POINT ( 'NONE',  ( -42.50000000000000000, 10.00000000000000000, 47.49999999999999289 ) ) ;
#3070 = ORIENTED_EDGE ( 'NONE', *, *, #3966, .F. ) ;
#3071 = CARTESIAN_POINT ( 'NONE',  ( 34.13396246814584600, -14.93538271375421900, -2.999999999999971578 ) ) ;
#3072 = AXIS2_PLACEMENT_3D ( 'NONE', #4866, #20225, #18842 ) ;
#3073 = DIRECTION ( 'NONE',  ( 0.000000000000000000, -0.000000000000000000, -1.000000000000000000 ) ) ;
#3074 = CARTESIAN_POINT ( 'NONE',  ( 35.00000000000000000, -9.000000000000001776, 4.258610482196280173E-15 ) ) ;
#3075 = DIRECTION ( 'NONE',  ( 1.000000000000000000, 0.000000000000000000, 0.000000000000000000 ) ) ;
#3076 = AXIS2_PLACEMENT_3D ( 'NONE', #17866, #5594, #7097 ) ;
#3077 = VERTEX_POINT ( 'NONE', #9876 ) ;
#3078 = ORIENTED_EDGE ( 'NONE', *, *, #21368, .F. ) ;
#3079 = FACE_OUTER_BOUND ( 'NONE', #16197, .T. ) ;
#3080 = EDGE_CURVE ( 'NONE', #9683, #17743, #10559, .T. ) ;
#3081 = AXIS2_PLACEMENT_3D ( 'NONE', #14799, #18600, #4627 ) ;
#3082 = DIRECTION ( 'NONE',  ( -0.000000000000000000, -0.000000000000000000, 1.000000000000000000 ) ) ;
#3083 = ORIENTED_EDGE ( 'NONE', *, *, #12925, .F. ) ;
#3084 = DIRECTION ( 'NONE',  ( -6.505213034913038160E-19, -3.903127820947822896E-18, -1.000000000000000000 ) ) ;
#3085 = AXIS2_PLACEMENT_3D ( 'NONE', #4024, #9509, #21544 ) ;
#3086 = FACE_OUTER_BOUND ( 'NONE', #6443, .T. ) ;
#3087 = CARTESIAN_POINT ( 'NONE',  ( -9.952189117650851458, 40.00000000000000000, -53.64426396172072486 ) ) ;
#3088 = CARTESIAN_POINT ( 'NONE',  ( -22.20997089757256049, 23.22761694305070534, -58.62102808997008907 ) ) ;
#3089 = CIRCLE ( 'NONE', #18441, 0.9999999999999995559 ) ;
#3090 = CARTESIAN_POINT ( 'NONE',  ( -0.7361830413879804080, 39.99998182960236193, 49.30709089395045197 ) ) ;
#3091 = CARTESIAN_POINT ( 'NONE',  ( -17.76087593031472522, 33.76750075041050536, 57.47290953699844351 ) ) ;
#3092 = EDGE_LOOP ( 'NONE', ( #20794, #13463 ) ) ;
#3093 = CARTESIAN_POINT ( 'NONE',  ( 13.08927703801864872, 27.36553638769444063, 44.94509734929667388 ) ) ;
#3094 = CARTESIAN_POINT ( 'NONE',  ( -35.00000000000058265, 40.00000000000000711, -55.00000000000076028 ) ) ;
#3095 = LINE ( 'NONE', #14993, #11566 ) ;
#3096 = DIRECTION ( 'NONE',  ( -0.000000000000000000, -0.000000000000000000, -1.000000000000000000 ) ) ;
#3097 = ORIENTED_EDGE ( 'NONE', *, *, #1333, .F. ) ;
#3098 = VECTOR ( 'NONE', #4298, 1000.000000000000000 ) ;
#3099 = DIRECTION ( 'NONE',  ( -1.000000000000000000, 0.000000000000000000, 0.000000000000000000 ) ) ;
#3100 = CARTESIAN_POINT ( 'NONE',  ( -17.86915608785656673, 27.01645732367835606, -6.999999999999992006 ) ) ;
#3101 = EDGE_CURVE ( 'NONE', #5844, #9303, #19375, .T. ) ;
#3102 = AXIS2_PLACEMENT_3D ( 'NONE', #20493, #18423, #16830 ) ;
#3103 = ORIENTED_EDGE ( 'NONE', *, *, #397, .F. ) ;
#3104 = EDGE_CURVE ( 'NONE', #2120, #12680, #21562, .T. ) ;
#3105 = EDGE_CURVE ( 'NONE', #22237, #10740, #7294, .T. ) ;
#3106 = ORIENTED_EDGE ( 'NONE', *, *, #10249, .T. ) ;
#3107 = ITEM_DEFINED_TRANSFORMATION ( 'NONE', 'NONE', #2916,  #18273 ) ;
#3108 = ORIENTED_EDGE ( 'NONE', *, *, #11411, .F. ) ;
#3109 = DIRECTION ( 'NONE',  ( 0.000000000000000000, 0.000000000000000000, -1.000000000000000000 ) ) ;
#3110 = CARTESIAN_POINT ( 'NONE',  ( 34.88850421923997658, -1.128083539116281342, -2.999999999999971578 ) ) ;
#3111 = FACE_OUTER_BOUND ( 'NONE', #22167, .T. ) ;
#3112 = CARTESIAN_POINT ( 'NONE',  ( 3.071904583821672593E-15, -4.500000000000010658, 0.000000000000000000 ) ) ;
#3113 = CARTESIAN_POINT ( 'NONE',  ( 20.00000000000041211, -2.750597533486379899E-14, -2.999999999999971578 ) ) ;
#3114 = ORIENTED_EDGE ( 'NONE', *, *, #17594, .T. ) ;
#3115 = CARTESIAN_POINT ( 'NONE',  ( -22.12933039895921183, 3.000000000000009326, 0.000000000000000000 ) ) ;
#3116 = CARTESIAN_POINT ( 'NONE',  ( -32.20238537491798780, -4.080045426412992171, 2.999999999999995559 ) ) ;
#3117 = ORIENTED_EDGE ( 'NONE', *, *, #14660, .F. ) ;
#3118 = LINE ( 'NONE', #13625, #20025 ) ;
#3119 = DIRECTION ( 'NONE',  ( 1.000000000000000000, 0.000000000000000000, 0.000000000000000000 ) ) ;
#3120 = AXIS2_PLACEMENT_3D ( 'NONE', #7065, #14032, #14149 ) ;
#3121 = PLANE ( 'NONE',  #6042 ) ;
#3122 = CARTESIAN_POINT ( 'NONE',  ( 9.689843208404314012, 39.33333333333335702, 54.54983754392762307 ) ) ;
#3123 = ORIENTED_EDGE ( 'NONE', *, *, #6032, .F. ) ;
#3124 = DIRECTION ( 'NONE',  ( 0.000000000000000000, 0.000000000000000000, 1.000000000000000000 ) ) ;
#3125 = ADVANCED_FACE ( 'NONE', ( #2673 ), #6219, .T. ) ;
#3126 = ORIENTED_EDGE ( 'NONE', *, *, #6887, .T. ) ;
#3127 = CARTESIAN_POINT ( 'NONE',  ( 14.74639653023263008, -28.96193690644938101, -2.999999999999971578 ) ) ;
#3128 = CARTESIAN_POINT ( 'NONE',  ( -20.10834676944521249, 10.02088872142242693, 58.12296025200766536 ) ) ;
#3129 = ORIENTED_EDGE ( 'NONE', *, *, #12487, .T. ) ;
#3130 = DIRECTION ( 'NONE',  ( 0.9898477157360406897, 0.000000000000000000, 0.1421319796954317316 ) ) ;
#3131 = DIRECTION ( 'NONE',  ( 0.000000000000000000, 0.000000000000000000, 1.000000000000000000 ) ) ;
#3132 = DIRECTION ( 'NONE',  ( 0.000000000000000000, 0.000000000000000000, -1.000000000000000000 ) ) ;
#3133 = AXIS2_PLACEMENT_3D ( 'NONE', #1968, #13974, #10551 ) ;
#3134 = EDGE_CURVE ( 'NONE', #9062, #12985, #18351, .T. ) ;
#3135 = AXIS2_PLACEMENT_3D ( 'NONE', #4136, #2647, #9289 ) ;
#3136 = CARTESIAN_POINT ( 'NONE',  ( 20.25803107563791983, 29.70716601075176300, -58.16264420749838138 ) ) ;
#3137 = AXIS2_PLACEMENT_3D ( 'NONE', #6785, #13748, #11817 ) ;
#3138 = VERTEX_POINT ( 'NONE', #828 ) ;
#3139 = B_SPLINE_CURVE_WITH_KNOTS ( 'NONE', 3,
 ( #22338, #18886, #15538, #8567, #3316, #22219 ),
 .UNSPECIFIED., .F., .F.,
 ( 4, 2, 4 ),
 ( 1.734723475976807094E-18, 0.003173601132114239540, 0.006347202264228477345 ),
 .UNSPECIFIED. ) ;
#3140 = AXIS2_PLACEMENT_3D ( 'NONE', #16818, #9493, #13351 ) ;
#3141 = EDGE_LOOP ( 'NONE', ( #611, #18493, #8514, #2194 ) ) ;
#3142 = ORIENTED_EDGE ( 'NONE', *, *, #8081, .T. ) ;
#3143 = B_SPLINE_CURVE_WITH_KNOTS ( 'NONE', 3,
 ( #16538, #20211, #840, #21819 ),
 .UNSPECIFIED., .F., .F.,
 ( 4, 4 ),
 ( 0.000000000000000000, 0.001452302087772874839 ),
 .UNSPECIFIED. ) ;
#3144 = EDGE_LOOP ( 'NONE', ( #333, #17242, #15002, #10659 ) ) ;
#3145 = CARTESIAN_POINT ( 'NONE',  ( -8.485281374238290653, -3.000000000000308198, -4.999999999999997335 ) ) ;
#3146 = FACE_OUTER_BOUND ( 'NONE', #13165, .T. ) ;
#3147 = DIRECTION ( 'NONE',  ( 0.000000000000000000, 0.000000000000000000, 1.000000000000000000 ) ) ;
#3148 = EDGE_LOOP ( 'NONE', ( #12892, #6241 ) ) ;
#3149 = CARTESIAN_POINT ( 'NONE',  ( -42.50000000000000711, -12.00000000000000000, -47.50000000000000000 ) ) ;
#3150 = CARTESIAN_POINT ( 'NONE',  ( -2.066061548966867889, -1.174227811081267614, -49.70141618117483517 ) ) ;
#3151 = VERTEX_POINT ( 'NONE', #22144 ) ;
#3152 = CIRCLE ( 'NONE', #17050, 15.00000000000000000 ) ;
#3153 = AXIS2_PLACEMENT_3D ( 'NONE', #8765, #7038, #48 ) ;
#3154 = AXIS2_PLACEMENT_3D ( 'NONE', #8531, #8978, #7380 ) ;
#3155 = ADVANCED_FACE ( 'NONE', ( #9765 ), #13404, .T. ) ;
#3156 = EDGE_LOOP ( 'NONE', ( #15749, #1531, #16740, #19176 ) ) ;
#3157 = CARTESIAN_POINT ( 'NONE',  ( 8.957608338236010326, 39.56964539817487037, -54.21301299504590077 ) ) ;
#3158 = LINE ( 'NONE', #10125, #6157 ) ;
#3159 = CARTESIAN_POINT ( 'NONE',  ( 6.696867368504048330E-15, 5.000000000000000888, 38.73397172404480671 ) ) ;
#3160 = CARTESIAN_POINT ( 'NONE',  ( -2.243248548005440046, 39.96968647079420123, 50.39828113659874731 ) ) ;
#3161 = AXIS2_PLACEMENT_3D ( 'NONE', #22565, #17265, #13584 ) ;
#3162 = EDGE_CURVE ( 'NONE', #6209, #12263, #7939, .T. ) ;
#3163 = EDGE_CURVE ( 'NONE', #17046, #6470, #17144, .T. ) ;
#3164 = ADVANCED_FACE ( 'NONE', ( #2783 ), #9475, .T. ) ;
#3165 = CARTESIAN_POINT ( 'NONE',  ( 8.916870955515532771, 2.080241304161451144, -56.50845996868347498 ) ) ;
#3166 = CIRCLE ( 'NONE', #7924, 2.500000000000002220 ) ;
#3167 = ORIENTED_EDGE ( 'NONE', *, *, #3026, .F. ) ;
#3168 = VECTOR ( 'NONE', #14054, 999.9999999999998863 ) ;
#3169 = ORIENTED_EDGE ( 'NONE', *, *, #9920, .T. ) ;
#3170 = EDGE_CURVE ( 'NONE', #15847, #19175, #19739, .T. ) ;
#3171 = EDGE_LOOP ( 'NONE', ( #3117, #19504, #7395, #8158 ) ) ;
#3172 = ORIENTED_EDGE ( 'NONE', *, *, #17176, .F. ) ;
#3173 = DIRECTION ( 'NONE',  ( -1.000000000000000000, 0.000000000000000000, 0.000000000000000000 ) ) ;
#3174 = AXIS2_PLACEMENT_3D ( 'NONE', #3756, #12999, #4437 ) ;
#3175 = DIRECTION ( 'NONE',  ( 6.505213034913038160E-19, 3.903127820947822896E-18, 1.000000000000000000 ) ) ;
#3176 = B_SPLINE_CURVE_WITH_KNOTS ( 'NONE', 3,
 ( #11857, #11636, #1106, #3165, #10132, #17124 ),
 .UNSPECIFIED., .F., .F.,
 ( 4, 2, 4 ),
 ( 0.000000000000000000, 0.002641318319677479071, 0.005282636639354958141 ),
 .UNSPECIFIED. ) ;
#3177 = EDGE_CURVE ( 'NONE', #9803, #10281, #19587, .T. ) ;
#3178 = DIRECTION ( 'NONE',  ( -0.000000000000000000, 1.000000000000000000, -0.000000000000000000 ) ) ;
#3179 = FACE_OUTER_BOUND ( 'NONE', #192, .T. ) ;
#3180 = EDGE_CURVE ( 'NONE', #2243, #15662, #14792, .T. ) ;
#3181 = ORIENTED_EDGE ( 'NONE', *, *, #6274, .T. ) ;
#3182 = FACE_OUTER_BOUND ( 'NONE', #18847, .T. ) ;
#3183 = CARTESIAN_POINT ( 'NONE',  ( -7.892682273998517850, 40.00000000000000000, -52.92195235550753551 ) ) ;
#3184 = CARTESIAN_POINT ( 'NONE',  ( 5.074925817841996256, -32.10132595304126824, -2.999999999999995559 ) ) ;
#3185 = DIRECTION ( 'NONE',  ( 0.000000000000000000, 1.000000000000000000, 0.000000000000000000 ) ) ;
#3186 = AXIS2_PLACEMENT_3D ( 'NONE', #21667, #5741, #9522 ) ;
#3187 = ORIENTED_EDGE ( 'NONE', *, *, #12577, .F. ) ;
#3188 = CARTESIAN_POINT ( 'NONE',  ( 42.50000000000000711, -12.00000000000012434, 44.97499999999989484 ) ) ;
#3189 = VECTOR ( 'NONE', #3945, 1000.000000000000114 ) ;
#3190 = ORIENTED_EDGE ( 'NONE', *, *, #1104, .T. ) ;
#3191 = FACE_OUTER_BOUND ( 'NONE', #838, .T. ) ;
#3192 = CARTESIAN_POINT ( 'NONE',  ( 0.000000000000000000, -45.00000000000000000, 0.000000000000000000 ) ) ;
#3193 = FACE_OUTER_BOUND ( 'NONE', #4822, .T. ) ;
#3194 = CARTESIAN_POINT ( 'NONE',  ( 5.093313992686365310, 32.09841355225992743, -6.999999999999999112 ) ) ;
#3195 = ADVANCED_FACE ( 'NONE', ( #2903 ), #9110, .F. ) ;
#3196 = EDGE_LOOP ( 'NONE', ( #19684, #11491, #11820, #18594 ) ) ;
#3197 = EDGE_CURVE ( 'NONE', #22134, #768, #14573, .T. ) ;
#3198 = AXIS2_PLACEMENT_3D ( 'NONE', #12267, #10539, #19046 ) ;
#3199 = AXIS2_PLACEMENT_3D ( 'NONE', #2389, #7885, #20037 ) ;
#3200 = ORIENTED_EDGE ( 'NONE', *, *, #6746, .F. ) ;
#3201 = DIRECTION ( 'NONE',  ( 6.505213034913038160E-19, 3.903127820947822896E-18, 1.000000000000000000 ) ) ;
#3202 = EDGE_CURVE ( 'NONE', #4584, #7707, #16799, .T. ) ;
#3203 = DIRECTION ( 'NONE',  ( 1.000000000000000000, 0.000000000000000000, 0.000000000000000000 ) ) ;
#3204 = EDGE_LOOP ( 'NONE', ( #1613, #11629, #3342, #12290 ) ) ;
#3205 = DIRECTION ( 'NONE',  ( 0.8171172023792930839, 0.3308262969259979092, 0.4720947350247287067 ) ) ;
#3206 = AXIS2_PLACEMENT_3D ( 'NONE', #16063, #3935, #17905 ) ;
#3207 = CARTESIAN_POINT ( 'NONE',  ( -28.50000000000001421, 19.99999999999982947, 60.00099999999999767 ) ) ;
#3208 = CARTESIAN_POINT ( 'NONE',  ( 0.000000000000000000, 30.00000000000000000, 0.000000000000000000 ) ) ;
#3209 = CARTESIAN_POINT ( 'NONE',  ( -20.89003165053261313, 11.75591475223743210, -58.31867307082492147 ) ) ;
#3210 = DIRECTION ( 'NONE',  ( 0.000000000000000000, 0.000000000000000000, 1.000000000000000000 ) ) ;
#3211 = AXIS2_PLACEMENT_3D ( 'NONE', #2448, #19517, #21237 ) ;
#3212 = CARTESIAN_POINT ( 'NONE',  ( -14.30127497006392012, 34.01755211514664978, 56.34491176086896047 ) ) ;
#3213 = EDGE_LOOP ( 'NONE', ( #17359, #9039 ) ) ;
#3214 = CARTESIAN_POINT ( 'NONE',  ( 29.99999999999998579, 20.00000000000000355, -105.0000000000000142 ) ) ;
#3215 = CIRCLE ( 'NONE', #2113, 11.00000000000003730 ) ;
#3216 = DIRECTION ( 'NONE',  ( 0.000000000000000000, 1.000000000000000000, 0.000000000000000000 ) ) ;
#3217 = CARTESIAN_POINT ( 'NONE',  ( 13.56354382738788367, 2.142135623730777372, -56.03997097393713034 ) ) ;
#3218 = CARTESIAN_POINT ( 'NONE',  ( -35.00000000000058265, 28.00000000000000000, -55.00000000000076028 ) ) ;
#3219 = EDGE_LOOP ( 'NONE', ( #15771, #11245, #13002, #1519 ) ) ;
#3220 = DIRECTION ( 'NONE',  ( 0.000000000000000000, 0.000000000000000000, 1.000000000000000000 ) ) ;
#3221 = LINE ( 'NONE', #10187, #216 ) ;
#3222 = CARTESIAN_POINT ( 'NONE',  ( 23.74488952252792728, -25.58633464742643326, 2.999999999999999112 ) ) ;
#3223 = DIRECTION ( 'NONE',  ( -6.505213034913038160E-19, -3.903127820947822896E-18, -1.000000000000000000 ) ) ;
#3224 = EDGE_CURVE ( 'NONE', #12952, #8904, #8491, .T. ) ;
#3225 = VECTOR ( 'NONE', #9664, 1000.000000000000000 ) ;
#3226 = ORIENTED_EDGE ( 'NONE', *, *, #14377, .F. ) ;
#3227 = CIRCLE ( 'NONE', #16011, 10.00000000000000178 ) ;
#3228 = AXIS2_PLACEMENT_3D ( 'NONE', #167, #15857, #7165 ) ;
#3229 = EDGE_LOOP ( 'NONE', ( #3200, #2312, #7838, #18951 ) ) ;
#3230 = CARTESIAN_POINT ( 'NONE',  ( 6.696867368503558448E-15, 0.000000000000000000, 48.73397172404481381 ) ) ;
#3231 = CARTESIAN_POINT ( 'NONE',  ( 2.220446049250313081E-13, -2.498001805406602216E-13, -6.859353255829918616 ) ) ;
#3232 = CARTESIAN_POINT ( 'NONE',  ( 32.10132595304135350, 5.074925817841719144, -7.000000000000006217 ) ) ;
#3233 = FACE_OUTER_BOUND ( 'NONE', #11673, .T. ) ;
#3234 = CARTESIAN_POINT ( 'NONE',  ( -32.35999952201571972, 1.423424233832654151, -7.000000000000006217 ) ) ;
#3235 = ORIENTED_EDGE ( 'NONE', *, *, #6400, .T. ) ;
#3236 = DIRECTION ( 'NONE',  ( -1.000000000000000000, -1.208970125616077665E-17, 0.000000000000000000 ) ) ;
#3237 = CARTESIAN_POINT ( 'NONE',  ( -27.19760187735852242, -24.73600648735135721, 2.800654218530492123 ) ) ;
#3238 = EDGE_LOOP ( 'NONE', ( #4771, #12071 ) ) ;
#3239 = CARTESIAN_POINT ( 'NONE',  ( -5.833333333333340143, 39.00000000000000711, -40.61164310337066041 ) ) ;
#3240 = EDGE_CURVE ( 'NONE', #5472, #968, #3575, .T. ) ;
#3241 = DIRECTION ( 'NONE',  ( 1.000000000000000000, 0.000000000000000000, 0.000000000000000000 ) ) ;
#3242 = CARTESIAN_POINT ( 'NONE',  ( -42.50000000000000711, -12.00000000000000000, -47.50000000000000000 ) ) ;
#3243 = CARTESIAN_POINT ( 'NONE',  ( 7.474679896992488359, 39.63145871420505273, 53.58934897198174241 ) ) ;
#3244 = EDGE_LOOP ( 'NONE', ( #15424, #19591 ) ) ;
#3245 = CARTESIAN_POINT ( 'NONE',  ( -36.75746821813305587, 0.6841746959065087008, -1.999999999999977573 ) ) ;
#3246 = AXIS2_PLACEMENT_3D ( 'NONE', #3071, #10042, #18882 ) ;
#3247 = ORIENTED_EDGE ( 'NONE', *, *, #19252, .F. ) ;
#3248 = DIRECTION ( 'NONE',  ( -0.000000000000000000, 1.000000000000000000, -0.000000000000000000 ) ) ;
#3249 = LINE ( 'NONE', #17207, #18456 ) ;
#3250 = ORIENTED_EDGE ( 'NONE', *, *, #5660, .T. ) ;
#3251 = CARTESIAN_POINT ( 'NONE',  ( 31.47514467962671247, -17.79500259159635078, 2.932460736555848602 ) ) ;
#3252 = EDGE_CURVE ( 'NONE', #10996, #10333, #13849, .T. ) ;
#3253 = AXIS2_PLACEMENT_3D ( 'NONE', #14800, #20096, #16180 ) ;
#3254 = CARTESIAN_POINT ( 'NONE',  ( 5.275737522157127195E-15, 12.49999999999999645, 0.000000000000000000 ) ) ;
#3255 = CARTESIAN_POINT ( 'NONE',  ( -31.57187188083505802, -7.711478842616608986, -2.999999999999971578 ) ) ;
#3256 = AXIS2_PLACEMENT_3D ( 'NONE', #9401, #16378, #14650 ) ;
#3257 = CYLINDRICAL_SURFACE ( 'NONE', #3822, 10.00000000000000000 ) ;
#3258 = EDGE_LOOP ( 'NONE', ( #279, #7361, #12926, #9656 ) ) ;
#3259 = VERTEX_POINT ( 'NONE', #3115 ) ;
#3260 = CIRCLE ( 'NONE', #5080, 2.099999999999990763 ) ;
#3261 = ORIENTED_EDGE ( 'NONE', *, *, #21083, .T. ) ;
#3262 = AXIS2_PLACEMENT_3D ( 'NONE', #1849, #1621, #6664 ) ;
#3263 = DIRECTION ( 'NONE',  ( -6.505213034913038160E-19, -3.903127820947822896E-18, -1.000000000000000000 ) ) ;
#3264 = ORIENTED_EDGE ( 'NONE', *, *, #2607, .T. ) ;
#3265 = CARTESIAN_POINT ( 'NONE',  ( -1.845281852317813165, 24.39721667535817673, 6.813359845952963845 ) ) ;
#3266 = CARTESIAN_POINT ( 'NONE',  ( -8.331955809010628045, 38.18181818181818699, 56.36098470834075158 ) ) ;
#3267 = CARTESIAN_POINT ( 'NONE',  ( -34.99999999999980815, 26.00000000000000355, 57.09999999999921982 ) ) ;
#3268 = VERTEX_POINT ( 'NONE', #6900 ) ;
#3269 = LINE ( 'NONE', #15614, #2866 ) ;
#3270 = LINE ( 'NONE', #12405, #4800 ) ;
#3271 = ORIENTED_EDGE ( 'NONE', *, *, #14496, .F. ) ;
#3272 = ADVANCED_FACE ( 'NONE', ( #15357 ), #10536, .T. ) ;
#3273 = AXIS2_PLACEMENT_3D ( 'NONE', #937, #13172, #7930 ) ;
#3274 = DIRECTION ( 'NONE',  ( -0.000000000000000000, -1.000000000000000000, -0.000000000000000000 ) ) ;
#3275 = DIRECTION ( 'NONE',  ( 0.000000000000000000, 0.000000000000000000, 1.000000000000000000 ) ) ;
#3276 = CARTESIAN_POINT ( 'NONE',  ( -32.20238537491819386, -4.080045426413020593, -2.999999999999975131 ) ) ;
#3277 = EDGE_LOOP ( 'NONE', ( #1288, #13989, #378, #15264, #15144, #18553 ) ) ;
#3278 = DIRECTION ( 'NONE',  ( -1.000000000000000000, 0.000000000000000000, 0.000000000000000000 ) ) ;
#3279 = CARTESIAN_POINT ( 'NONE',  ( -42.50000000000000711, -12.00000000000012434, 47.50000000000000711 ) ) ;
#3280 = CARTESIAN_POINT ( 'NONE',  ( 89.99999999999701572, 0.000000000000000000, -5.216535399428728743E-14 ) ) ;
#3281 = CARTESIAN_POINT ( 'NONE',  ( -0.9695481421535360189, 39.99443253533478781, 49.47361716149077182 ) ) ;
#3282 = EDGE_CURVE ( 'NONE', #6865, #17042, #10930, .T. ) ;
#3283 = CIRCLE ( 'NONE', #18637, 25.00000000000000000 ) ;
#3284 = FACE_OUTER_BOUND ( 'NONE', #20720, .T. ) ;
#3285 = CIRCLE ( 'NONE', #2540, 34.90673715956759082 ) ;
#3286 = CARTESIAN_POINT ( 'NONE',  ( -20.17230487860815913, -25.34312177887351680, -2.999999999999995559 ) ) ;
#3287 = ORIENTED_EDGE ( 'NONE', *, *, #3841, .F. ) ;
#3288 = ORIENTED_EDGE ( 'NONE', *, *, #19075, .F. ) ;
#3289 = EDGE_CURVE ( 'NONE', #7701, #21800, #20982, .T. ) ;
#3290 = ORIENTED_EDGE ( 'NONE', *, *, #2954, .F. ) ;
#3291 = ORIENTED_EDGE ( 'NONE', *, *, #10893, .F. ) ;
#3292 = CARTESIAN_POINT ( 'NONE',  ( 2.854018578421813982E-15, -6.180736333215565814, 0.000000000000000000 ) ) ;
#3293 = DIRECTION ( 'NONE',  ( -1.000000000000000000, -1.208970125616063644E-17, 0.000000000000000000 ) ) ;
#3294 = AXIS2_PLACEMENT_3D ( 'NONE', #17858, #14052, #207 ) ;
#3295 = LINE ( 'NONE', #19440, #19357 ) ;
#3296 = CARTESIAN_POINT ( 'NONE',  ( -90.00000000000000000, 40.00000000000000711, -9.108981535246192915E-16 ) ) ;
#3297 = CARTESIAN_POINT ( 'NONE',  ( -11.85142133643352480, 40.00000000000000711, 54.27688992489014908 ) ) ;
#3298 = EDGE_CURVE ( 'NONE', #21800, #16, #21928, .T. ) ;
#3299 = ADVANCED_FACE ( 'NONE', ( #22261 ), #20829, .T. ) ;
#3300 = ORIENTED_EDGE ( 'NONE', *, *, #14528, .F. ) ;
#3301 = CARTESIAN_POINT ( 'NONE',  ( -34.64554704988852052, -10.35112103033883812, -2.932164912090537534 ) ) ;
#3302 = CARTESIAN_POINT ( 'NONE',  ( -8.540030425000768588, 39.99999999999998579, -53.17106805020448945 ) ) ;
#3303 = LINE ( 'NONE', #1341, #273 ) ;
#3304 = DIRECTION ( 'NONE',  ( 1.000000000000000000, 0.000000000000000000, 0.000000000000000000 ) ) ;
#3305 = FACE_OUTER_BOUND ( 'NONE', #5612, .T. ) ;
#3306 = AXIS2_PLACEMENT_3D ( 'NONE', #14186, #21200, #12471 ) ;
#3307 =( BOUNDED_SURFACE ( )  B_SPLINE_SURFACE ( 3, 2, ( 
 ( #12972, #2573, #18364 ),
 ( #4632, #11610, #18605 ),
 ( #841, #18262, #16539 ),
 ( #2684, #9890, #7830 ),
 ( #1079, #7951, #8067 ),
 ( #14913, #9662, #21940 ),
 ( #20440, #18715, #16880 ),
 ( #8172, #6232, #6789 ) ),
 .UNSPECIFIED., .F., .F., .F. ) 
 B_SPLINE_SURFACE_WITH_KNOTS ( ( 4, 2, 2, 4 ),
 ( 3, 3 ),
 ( 0.000000000000000000, 0.005619275362615350038, 0.008428913043923024623, 0.01123855072523070008 ),
 ( 0.000000000000000000, 1.000000000000000000 ),
 .UNSPECIFIED. ) 
 GEOMETRIC_REPRESENTATION_ITEM ( )  RATIONAL_B_SPLINE_SURFACE ( (
 ( 1.000000000000000000, 0.7200096751079133606, 1.000000000000000000),
 ( 1.000000000000000000, 0.7496867072825520451, 1.000000000000000000),
 ( 1.000000000000000000, 0.7737790075298972559, 1.000000000000000000),
 ( 1.000000000000000000, 0.8024253043749317582, 1.000000000000000000),
 ( 1.000000000000000000, 0.8107149009171402687, 1.000000000000000000),
 ( 1.000000000000000000, 0.8248887618771173491, 1.000000000000000000),
 ( 1.000000000000000000, 0.8307759608768628956, 1.000000000000000000),
 ( 1.000000000000000000, 0.8354972831517065712, 1.000000000000000000) ) ) 
 REPRESENTATION_ITEM ( '' )  SURFACE ( )  );
#3308 = ORIENTED_EDGE ( 'NONE', *, *, #357, .T. ) ;
#3309 = EDGE_CURVE ( 'NONE', #22647, #15500, #14945, .T. ) ;
#3310 = PLANE ( 'NONE',  #8420 ) ;
#3311 = EDGE_LOOP ( 'NONE', ( #5449, #14473 ) ) ;
#3312 = FACE_OUTER_BOUND ( 'NONE', #20333, .T. ) ;
#3313 = CARTESIAN_POINT ( 'NONE',  ( 42.50000000000000711, -12.00000000000000000, -47.50000000000000000 ) ) ;
#3314 = CIRCLE ( 'NONE', #14983, 19.99999999999999289 ) ;
#3315 = CARTESIAN_POINT ( 'NONE',  ( -31.92986134326225667, 18.22261011550274645, 2.800654218530509443 ) ) ;
#3316 = CARTESIAN_POINT ( 'NONE',  ( -1.072795092646378734, 35.00000000000000000, 38.73397172404480671 ) ) ;
#3317 = EDGE_CURVE ( 'NONE', #4351, #21949, #14, .T. ) ;
#3318 = ORIENTED_EDGE ( 'NONE', *, *, #5798, .T. ) ;
#3319 = EDGE_CURVE ( 'NONE', #14813, #6131, #1064, .T. ) ;
#3320 = ORIENTED_EDGE ( 'NONE', *, *, #9372, .T. ) ;
#3321 = CARTESIAN_POINT ( 'NONE',  ( 5.551115123125782702E-14, -1.387778780781445676E-13, -5.749999999999949374 ) ) ;
#3322 = TOROIDAL_SURFACE ( 'NONE', #16104, 34.90673715956759082, 8.750000000000000000 ) ;
#3323 = CARTESIAN_POINT ( 'NONE',  ( 2.775557561562891351E-14, -2.775557561562891351E-14, 2.999999999999999112 ) ) ;
#3324 = EDGE_CURVE ( 'NONE', #19833, #16523, #17891, .T. ) ;
#3325 = EDGE_LOOP ( 'NONE', ( #14607, #3483, #8538, #18494, #14886 ) ) ;
#3326 = DIRECTION ( 'NONE',  ( 1.000000000000000000, 0.000000000000000000, 0.000000000000000000 ) ) ;
#3327 = LINE ( 'NONE', #6750, #20585 ) ;
#3328 = CARTESIAN_POINT ( 'NONE',  ( 0.000000000000000000, 30.00000000000000000, -7.500000000000000000 ) ) ;
#3329 = CARTESIAN_POINT ( 'NONE',  ( -20.00424115936587199, 19.83711385861052889, -60.62278039730740886 ) ) ;
#3330 = ADVANCED_FACE ( 'NONE', ( #20876 ), #2905, .F. ) ;
#3331 = CARTESIAN_POINT ( 'NONE',  ( -34.99999999999999289, -5.000000000000000000, -3.012171160963566127E-14 ) ) ;
#3332 = ORIENTED_EDGE ( 'NONE', *, *, #6770, .F. ) ;
#3333 = CARTESIAN_POINT ( 'NONE',  ( -12.99999999999980282, -2.516660498395516310, -105.0010000000000048 ) ) ;
#3334 = CARTESIAN_POINT ( 'NONE',  ( 12.00000000000000711, 28.19616000222403684, 1.469576158976823947E-15 ) ) ;
#3335 = EDGE_CURVE ( 'NONE', #11258, #2243, #6559, .T. ) ;
#3336 = FACE_BOUND ( 'NONE', #1977, .T. ) ;
#3337 = CARTESIAN_POINT ( 'NONE',  ( -35.28654656445755933, -4.153516728484126119, 3.000000000000047962 ) ) ;
#3338 = ORIENTED_EDGE ( 'NONE', *, *, #9562, .T. ) ;
#3339 = CIRCLE ( 'NONE', #11005, 18.00000000000000000 ) ;
#3340 = LINE ( 'NONE', #18571, #11181 ) ;
#3341 = CARTESIAN_POINT ( 'NONE',  ( 16.56444186175090749, -26.79308242454919764, -2.999999999999999112 ) ) ;
#3342 = ORIENTED_EDGE ( 'NONE', *, *, #9694, .F. ) ;
#3343 = APPLICATION_PROTOCOL_DEFINITION ( 'draft international standard', 'automotive_design', 1998, #7112 ) ;
#3344 = ORIENTED_EDGE ( 'NONE', *, *, #4142, .F. ) ;
#3345 = DIRECTION ( 'NONE',  ( 6.505213034913038160E-19, 3.903127820947822896E-18, 1.000000000000000000 ) ) ;
#3346 = CARTESIAN_POINT ( 'NONE',  ( 0.7217013449060836194, -4.626342591398014292, 46.01887142923336427 ) ) ;
#3347 = CYLINDRICAL_SURFACE ( 'NONE', #13196, 8.999999999999998224 ) ;
#3348 = CARTESIAN_POINT ( 'NONE',  ( -1.387778780781445518E-14, 20.00000000000000355, 100.0000000000000000 ) ) ;
#3349 = ORIENTED_EDGE ( 'NONE', *, *, #2294, .T. ) ;
#3350 = DIRECTION ( 'NONE',  ( 6.505213034913038160E-19, 3.903127820947822896E-18, 1.000000000000000000 ) ) ;
#3351 = CARTESIAN_POINT ( 'NONE',  ( -11.87329829276355042, 39.99999999999998579, 54.28004929203131468 ) ) ;
#3352 = ORIENTED_EDGE ( 'NONE', *, *, #18266, .T. ) ;
#3353 = LINE ( 'NONE', #3239, #14138 ) ;
#3354 = ADVANCED_FACE ( 'NONE', ( #1738 ), #13520, .T. ) ;
#3355 = CARTESIAN_POINT ( 'NONE',  ( -10.39230484541300825, -1.500000000000011768, -6.000000000000442313 ) ) ;
#3356 = DIRECTION ( 'NONE',  ( 0.8391477167891899791, 0.3845457931435842802, 0.3846500258456529431 ) ) ;
#3357 = LINE ( 'NONE', #1627, #2029 ) ;
#3358 = CARTESIAN_POINT ( 'NONE',  ( 10.38220159744132509, 30.85082733156617607, -43.52345836121336475 ) ) ;
#3359 = EDGE_LOOP ( 'NONE', ( #5325, #9602, #14619, #14769 ) ) ;
#3360 = DIRECTION ( 'NONE',  ( 1.445602896647339163E-16, 0.000000000000000000, 1.000000000000000000 ) ) ;
#3361 = DIRECTION ( 'NONE',  ( -0.000000000000000000, -1.000000000000000000, -0.000000000000000000 ) ) ;
#3362 = ORIENTED_EDGE ( 'NONE', *, *, #549, .F. ) ;
#3363 = CARTESIAN_POINT ( 'NONE',  ( 6.383438919230843859E-14, -25.00000000000000000, -20.00000000000029488 ) ) ;
#3364 = CIRCLE ( 'NONE', #22017, 10.00000000000000178 ) ;
#3365 = EDGE_CURVE ( 'NONE', #7282, #14700, #4838, .T. ) ;
#3366 = DIRECTION ( 'NONE',  ( -0.000000000000000000, 1.000000000000000000, -0.000000000000000000 ) ) ;
#3367 = CARTESIAN_POINT ( 'NONE',  ( 7.310544252644470693E-15, 28.19616000222403684, 0.000000000000000000 ) ) ;
#3368 = CARTESIAN_POINT ( 'NONE',  ( -90.00000000000000000, 26.00000000000000355, -2.099999999999991651 ) ) ;
#3369 = ORIENTED_EDGE ( 'NONE', *, *, #11016, .F. ) ;
#3370 = EDGE_LOOP ( 'NONE', ( #18621, #9458 ) ) ;
#3371 = VERTEX_POINT ( 'NONE', #13961 ) ;
#3372 = DIRECTION ( 'NONE',  ( 0.000000000000000000, 0.000000000000000000, 1.000000000000000000 ) ) ;
#3373 = ORIENTED_EDGE ( 'NONE', *, *, #9001, .T. ) ;
#3374 = CARTESIAN_POINT ( 'NONE',  ( -2.900269772763596876, 22.78549972664023215, 6.519988159899003932 ) ) ;
#3375 = CARTESIAN_POINT ( 'NONE',  ( 22.39119123459438043, 18.77992731964035755, 58.66020055843083014 ) ) ;
#3376 = EDGE_CURVE ( 'NONE', #3870, #9197, #12264, .T. ) ;
#3377 = VECTOR ( 'NONE', #581, 1000.000000000000000 ) ;
#3378 = CARTESIAN_POINT ( 'NONE',  ( -25.00000000000000000, 20.00000000000000000, 6.487780019669002523E-15 ) ) ;
#3379 = VERTEX_POINT ( 'NONE', #22376 ) ;
#3380 = CARTESIAN_POINT ( 'NONE',  ( 42.49999999999998579, 10.00000000000000000, -47.49999999999997868 ) ) ;
#3381 = FACE_OUTER_BOUND ( 'NONE', #9789, .T. ) ;
#3382 = ORIENTED_EDGE ( 'NONE', *, *, #8745, .F. ) ;
#3383 = EDGE_LOOP ( 'NONE', ( #9239, #2437, #2685, #17262 ) ) ;
#3384 = CARTESIAN_POINT ( 'NONE',  ( 1.838758599476162825, 34.88915224291387318, 38.90097524723616829 ) ) ;
#3385 = ORIENTED_EDGE ( 'NONE', *, *, #39, .F. ) ;
#3386 = CARTESIAN_POINT ( 'NONE',  ( 5.905685660495028522, 39.12130596110461767, -53.51375433846526875 ) ) ;
#3387 = DIRECTION ( 'NONE',  ( 0.000000000000000000, 0.000000000000000000, -1.000000000000000000 ) ) ;
#3388 = CARTESIAN_POINT ( 'NONE',  ( -4.557459432784731312, 39.87073546004029367, 51.93758234736819190 ) ) ;
#3389 = B_SPLINE_CURVE_WITH_KNOTS ( 'NONE', 3,
 ( #11603, #16418, #21695, #6448 ),
 .UNSPECIFIED., .F., .F.,
 ( 4, 4 ),
 ( 0.001893031756885525489, 0.003808480026563626671 ),
 .UNSPECIFIED. ) ;
#3390 = CARTESIAN_POINT ( 'NONE',  ( 13.56354382738799558, 2.142135623730931471, 56.03997097393685323 ) ) ;
#3391 = DIRECTION ( 'NONE',  ( 6.505213034913038160E-19, 3.903127820947822896E-18, 1.000000000000000000 ) ) ;
#3392 = AXIS2_PLACEMENT_3D ( 'NONE', #15750, #60, #7052 ) ;
#3393 = CARTESIAN_POINT ( 'NONE',  ( 22.22891329980544839, -23.65408649739131164, 3.000000000000023537 ) ) ;
#3395 = ORIENTED_EDGE ( 'NONE', *, *, #12725, .F. ) ;
#3394 = EDGE_CURVE ( 'NONE', #10477, #4282, #13621, .T. ) ;
#3396 = PRODUCT_RELATED_PRODUCT_CATEGORY ( 'part', '', ( #5829 ) ) ;
#3397 = ORIENTED_EDGE ( 'NONE', *, *, #8346, .F. ) ;
#3398 = VERTEX_POINT ( 'NONE', #16139 ) ;
#3399 = VERTEX_POINT ( 'NONE', #11106 ) ;
#3400 = CARTESIAN_POINT ( 'NONE',  ( -13.03660953228011010, 4.807999378483081898, 58.46122805341369855 ) ) ;
#3401 = EDGE_CURVE ( 'NONE', #7, #1985, #4720, .T. ) ;
#3402 = CARTESIAN_POINT ( 'NONE',  ( -8.485281374238564212, 12.49999999999999822, -3.000000000000000000 ) ) ;
#3403 = CARTESIAN_POINT ( 'NONE',  ( 42.50000000000000711, -9.600000000000001421, 47.50000000000000711 ) ) ;
#3404 = CARTESIAN_POINT ( 'NONE',  ( -12.99999999999980282, -2.516660498395516310, -100.0000000000000000 ) ) ;
#3405 = CARTESIAN_POINT ( 'NONE',  ( 1.076296735955945660, 39.99310909908677303, 49.55311975943427427 ) ) ;
#3406 = CIRCLE ( 'NONE', #11030, 10.00000000000000178 ) ;
#3407 = ORIENTED_EDGE ( 'NONE', *, *, #12251, .F. ) ;
#3408 = DIRECTION ( 'NONE',  ( 0.000000000000000000, 0.000000000000000000, 1.000000000000000000 ) ) ;
#3409 = CARTESIAN_POINT ( 'NONE',  ( -5.708997464095411090, 39.99999999999998579, -51.95724526860413306 ) ) ;
#3410 = DIRECTION ( 'NONE',  ( 0.000000000000000000, 1.000000000000000000, 0.000000000000000000 ) ) ;
#3411 = CARTESIAN_POINT ( 'NONE',  ( 7.505578006071305985, 1.461761173326671104, 55.63523492903841117 ) ) ;
#3412 = EDGE_CURVE ( 'NONE', #21198, #18097, #8734, .T. ) ;
#3413 = VERTEX_POINT ( 'NONE', #19385 ) ;
#3414 = CARTESIAN_POINT ( 'NONE',  ( 42.50000000000000711, -12.00000000000012434, -47.50000000000000000 ) ) ;
#3415 = VERTEX_POINT ( 'NONE', #5850 ) ;
#3416 = CARTESIAN_POINT ( 'NONE',  ( -7.555723902515834922, 38.52224445567419764, 55.93227658743229114 ) ) ;
#3417 = DIRECTION ( 'NONE',  ( -6.505213034913038160E-19, -3.903127820947822896E-18, -1.000000000000000000 ) ) ;
#3418 = FACE_BOUND ( 'NONE', #12714, .T. ) ;
#3419 = ADVANCED_FACE ( 'NONE', ( #10639, #10997, #21097, #21428, #1951, #12818, #7563, #10877, #5396 ), #19830, .F. ) ;
#3420 = ORIENTED_EDGE ( 'NONE', *, *, #22107, .T. ) ;
#3421 = AXIS2_PLACEMENT_3D ( 'NONE', #7622, #19663, #2127 ) ;
#3422 = ORIENTED_EDGE ( 'NONE', *, *, #2861, .T. ) ;
#3423 = VECTOR ( 'NONE', #10978, 1000.000000000000000 ) ;
#3424 = AXIS2_PLACEMENT_3D ( 'NONE', #2687, #8176, #22160 ) ;
#3425 = ORIENTED_EDGE ( 'NONE', *, *, #16886, .T. ) ;
#3426 = DIRECTION ( 'NONE',  ( -6.505213034913038160E-19, -3.903127820947822896E-18, -1.000000000000000000 ) ) ;
#3427 = DIRECTION ( 'NONE',  ( -1.000000000000000000, 0.000000000000000000, 0.000000000000000000 ) ) ;
#3428 = ORIENTED_EDGE ( 'NONE', *, *, #1467, .T. ) ;
#3429 = CARTESIAN_POINT ( 'NONE',  ( 13.07600923154786088, 12.64060470162857364, 44.93756990742568291 ) ) ;
#3430 = SHAPE_REPRESENTATION ( 'ROTARY LOBE', ( #18273 ), #17150 ) ;
#3431 = DIRECTION ( 'NONE',  ( 0.000000000000000000, 1.000000000000000000, 0.000000000000000000 ) ) ;
#3432 = CARTESIAN_POINT ( 'NONE',  ( -1.387778780781445518E-14, 20.00000000000000355, 103.0000000000000284 ) ) ;
#3433 = CARTESIAN_POINT ( 'NONE',  ( -16.49514046905042264, 8.656442121909590171, -59.66722042020315087 ) ) ;
#3434 = CARTESIAN_POINT ( 'NONE',  ( -33.52953626616041305, -9.708269511265326557, -2.999999999999971578 ) ) ;
#3435 = CONICAL_SURFACE ( 'NONE', #9279, 49.99999999999998579, 0.7853981633974657095 ) ;
#3436 = EDGE_CURVE ( 'NONE', #2840, #5633, #16413, .T. ) ;
#3437 = VERTEX_POINT ( 'NONE', #2413 ) ;
#3438 = DIRECTION ( 'NONE',  ( 1.000000000000000000, 0.000000000000000000, 0.000000000000000000 ) ) ;
#3439 = FACE_BOUND ( 'NONE', #5934, .T. ) ;
#3440 = CARTESIAN_POINT ( 'NONE',  ( -27.01645732367838448, -17.86915608785691489, 2.999999999999995559 ) ) ;
#3441 = AXIS2_PLACEMENT_3D ( 'NONE', #210, #7322, #9038 ) ;
#3442 = LINE ( 'NONE', #5489, #974 ) ;
#3443 = DIRECTION ( 'NONE',  ( -0.000000000000000000, 1.000000000000000000, -0.000000000000000000 ) ) ;
#3444 = VECTOR ( 'NONE', #1153, 1000.000000000000000 ) ;
#3445 = ORIENTED_EDGE ( 'NONE', *, *, #21208, .F. ) ;
#3446 = PLANE ( 'NONE',  #9367 ) ;
#3447 = DIRECTION ( 'NONE',  ( 6.505213034913038160E-19, 3.903127820947822896E-18, 1.000000000000000000 ) ) ;
#3448 = EDGE_CURVE ( 'NONE', #12800, #13841, #11298, .T. ) ;
#3449 = EDGE_CURVE ( 'NONE', #17215, #17302, #14201, .T. ) ;
#3450 = CIRCLE ( 'NONE', #12919, 51.00000000000001421 ) ;
#3451 = ORIENTED_EDGE ( 'NONE', *, *, #8194, .F. ) ;
#3452 = AXIS2_PLACEMENT_3D ( 'NONE', #9395, #4360, #4237 ) ;
#3453 = EDGE_CURVE ( 'NONE', #19820, #11397, #21540, .T. ) ;
#3454 = SHAPE_DEFINITION_REPRESENTATION ( #16821, #13507 ) ;
#3455 = CIRCLE ( 'NONE', #8931, 41.00000000000000000 ) ;
#3456 = ORIENTED_EDGE ( 'NONE', *, *, #10987, .T. ) ;
#3457 = DIRECTION ( 'NONE',  ( 1.296372316667914327E-16, 1.000000000000000000, -0.000000000000000000 ) ) ;
#3458 = DIRECTION ( 'NONE',  ( -6.505213034913038160E-19, -3.903127820947822896E-18, -1.000000000000000000 ) ) ;
#3459 = DIRECTION ( 'NONE',  ( 0.000000000000000000, 0.000000000000000000, -1.000000000000000000 ) ) ;
#3460 = DIRECTION ( 'NONE',  ( 0.000000000000000000, -1.000000000000000000, 0.000000000000000000 ) ) ;
#3461 = CARTESIAN_POINT ( 'NONE',  ( 12.99999999999993960, 42.51666049839543149, 100.0000000000000000 ) ) ;
#3462 = ORIENTED_EDGE ( 'NONE', *, *, #12562, .T. ) ;
#3463 = DIRECTION ( 'NONE',  ( -0.000000000000000000, -1.000000000000000000, -0.000000000000000000 ) ) ;
#3464 = CARTESIAN_POINT ( 'NONE',  ( 22.98755168577423902, 22.97438720605746099, -2.999999999999971578 ) ) ;
#3465 = ORIENTED_EDGE ( 'NONE', *, *, #4547, .T. ) ;
#3466 = CARTESIAN_POINT ( 'NONE',  ( 3.235223465815040278, -4.647308930658603288, -47.76313845446085793 ) ) ;
#3467 = DIRECTION ( 'NONE',  ( 1.296372316667914327E-16, 1.000000000000000000, -0.000000000000000000 ) ) ;
#3468 = CARTESIAN_POINT ( 'NONE',  ( 5.833333333333339255, 6.180730040185842711, 40.61164310337068173 ) ) ;
#3469 = CARTESIAN_POINT ( 'NONE',  ( 4.171001175319766219, 35.79662727779869869, -2.999999999999992450 ) ) ;
#3470 = DIRECTION ( 'NONE',  ( 6.505213034913038160E-19, 3.903127820947822896E-18, 1.000000000000000000 ) ) ;
#3471 = ORIENTED_EDGE ( 'NONE', *, *, #16678, .T. ) ;
#3472 = FACE_OUTER_BOUND ( 'NONE', #13417, .T. ) ;
#3473 = AXIS2_PLACEMENT_3D ( 'NONE', #9453, #503, #21364 ) ;
#3474 = CARTESIAN_POINT ( 'NONE',  ( -42.50000000000000711, -5.000000000000000000, 49.60000000000000853 ) ) ;
#3475 = ORIENTED_EDGE ( 'NONE', *, *, #2296, .F. ) ;
#3476 = DIRECTION ( 'NONE',  ( 6.505213034913038160E-19, 3.903127820947822896E-18, 1.000000000000000000 ) ) ;
#3477 = FACE_OUTER_BOUND ( 'NONE', #6339, .T. ) ;
#3478 = DIRECTION ( 'NONE',  ( -1.000000000000000000, 0.000000000000000000, 0.000000000000000000 ) ) ;
#3479 = B_SPLINE_CURVE_WITH_KNOTS ( 'NONE', 3,
 ( #8703, #8475, #22242, #12140 ),
 .UNSPECIFIED., .F., .F.,
 ( 4, 4 ),
 ( 9.545285770338856966E-07, 0.001900595205834574144 ),
 .UNSPECIFIED. ) ;
#3481 = ADVANCED_FACE ( 'NONE', ( #2182 ), #12706, .T. ) ;
#3480 = ORIENTED_EDGE ( 'NONE', *, *, #19931, .F. ) ;
#3482 = ADVANCED_FACE ( 'NONE', ( #10754 ), #19600, .T. ) ;
#3483 = ORIENTED_EDGE ( 'NONE', *, *, #3782, .F. ) ;
#3484 = CLOSED_SHELL ( 'NONE', ( #18863, #5857, #19734, #13310, #7530, #19685, #18289, #19085, #21947, #10343, #10632, #16278, #3272, #14244, #20666, #16635, #19070, #18858, #14622, #18536, #12603, #19793, #5819 ) ) ;
#3485 = EDGE_LOOP ( 'NONE', ( #8615, #10110, #2918, #13373 ) ) ;
#3486 = EDGE_LOOP ( 'NONE', ( #20263, #6307, #6714, #22054 ) ) ;
#3487 = FACE_OUTER_BOUND ( 'NONE', #1131, .T. ) ;
#3488 = CIRCLE ( 'NONE', #20671, 57.07106781186551103 ) ;
#3489 = CARTESIAN_POINT ( 'NONE',  ( 14.98269809772825489, 3.197274675470657357, 56.58282704237544891 ) ) ;
#3490 = CARTESIAN_POINT ( 'NONE',  ( -12.99999999999999289, 20.00000000000000000, 11.32475165290611940 ) ) ;
#3491 = CARTESIAN_POINT ( 'NONE',  ( 8.910373529401164561, 39.99999999999999289, 53.30647735977077417 ) ) ;
#3492 = EDGE_CURVE ( 'NONE', #8659, #11088, #9060, .T. ) ;
#3493 = ORIENTED_EDGE ( 'NONE', *, *, #14239, .T. ) ;
#3494 = FACE_BOUND ( 'NONE', #18429, .T. ) ;
#3495 = CARTESIAN_POINT ( 'NONE',  ( 0.05567163769005373242, -4.650449146058893923, -45.38800358221575948 ) ) ;
#3496 = VERTEX_POINT ( 'NONE', #14304 ) ;
#3497 = CARTESIAN_POINT ( 'NONE',  ( 34.99999999999980815, 40.00000000000000711, 52.47499999999922693 ) ) ;
#3498 = ORIENTED_EDGE ( 'NONE', *, *, #5104, .F. ) ;
#3499 = CARTESIAN_POINT ( 'NONE',  ( 35.00000000000058265, 26.00000000000000355, -52.90000000000076597 ) ) ;
#3500 = EDGE_LOOP ( 'NONE', ( #2831, #8629, #10943, #13779 ) ) ;
#3501 = CARTESIAN_POINT ( 'NONE',  ( 0.6290164960677582240, 40.00000000000000000, -49.48738346576788416 ) ) ;
#3502 = CIRCLE ( 'NONE', #16280, 31.50000000000000711 ) ;
#3503 = DIRECTION ( 'NONE',  ( 1.296372316667914327E-16, 1.000000000000000000, -0.000000000000000000 ) ) ;
#3504 = CARTESIAN_POINT ( 'NONE',  ( -2.105491371362254949, 39.97335800984880194, 50.30091810999239499 ) ) ;
#3505 = AXIS2_PLACEMENT_3D ( 'NONE', #19466, #7315, #8913 ) ;
#3506 = CARTESIAN_POINT ( 'NONE',  ( 0.6841746959068417677, 36.75746821813288534, -1.999999999999977573 ) ) ;
#3507 = CARTESIAN_POINT ( 'NONE',  ( 42.49999999999998579, 10.00000000000000000, -44.99999999999997868 ) ) ;
#3508 = VECTOR ( 'NONE', #5185, 1000.000000000000000 ) ;
#3509 = DIRECTION ( 'NONE',  ( 0.000000000000000000, 0.000000000000000000, -1.000000000000000000 ) ) ;
#3510 = EDGE_LOOP ( 'NONE', ( #719, #13213, #13948, #8055 ) ) ;
#3511 = EDGE_LOOP ( 'NONE', ( #18181, #22428, #18359, #11116 ) ) ;
#3512 = ORIENTED_EDGE ( 'NONE', *, *, #1374, .T. ) ;
#3513 = AXIS2_PLACEMENT_3D ( 'NONE', #16509, #7799, #5748 ) ;
#3514 = VECTOR ( 'NONE', #14344, 1000.000000000000000 ) ;
#3515 = ORIENTED_EDGE ( 'NONE', *, *, #5686, .F. ) ;
#3516 = CARTESIAN_POINT ( 'NONE',  ( 28.88846368933348074, 19.59430950039314823, 2.999999999999995559 ) ) ;
#3517 = DIRECTION ( 'NONE',  ( 0.000000000000000000, -0.5150380749100547106, -0.8571673007021120005 ) ) ;
#3518 = AXIS2_PLACEMENT_3D ( 'NONE', #18049, #2822, #4430 ) ;
#3519 = DIRECTION ( 'NONE',  ( -1.000000000000000000, 1.264902534566421922E-16, 0.000000000000000000 ) ) ;
#3520 = CARTESIAN_POINT ( 'NONE',  ( 8.331955809010601399, 38.18181818181818699, 56.36098470834073026 ) ) ;
#3521 = VECTOR ( 'NONE', #15900, 1000.000000000000000 ) ;
#3522 = CARTESIAN_POINT ( 'NONE',  ( 1.092487586117354859, 39.99289797745701236, 49.56515079790309386 ) ) ;
#3523 = VECTOR ( 'NONE', #21160, 1000.000000000000000 ) ;
#3524 = ORIENTED_EDGE ( 'NONE', *, *, #4411, .F. ) ;
#3525 = DIRECTION ( 'NONE',  ( 0.000000000000000000, 1.000000000000000000, -0.000000000000000000 ) ) ;
#3526 = CARTESIAN_POINT ( 'NONE',  ( -9.260192196558032052, 40.00000000000000000, -53.42688922523713302 ) ) ;
#3527 = CARTESIAN_POINT ( 'NONE',  ( 12.84899528830092130, 2.142135623730915039, -57.90797000640139913 ) ) ;
#3528 = B_SPLINE_CURVE_WITH_KNOTS ( 'NONE', 3,
 ( #6847, #8220, #1223, #11762 ),
 .UNSPECIFIED., .F., .F.,
 ( 4, 4 ),
 ( 0.000000000000000000, 0.001452302087772880043 ),
 .UNSPECIFIED. ) ;
#3529 = CARTESIAN_POINT ( 'NONE',  ( -42.50000000000000000, 10.00000000000000000, 47.49999999999999289 ) ) ;
#3530 = DIRECTION ( 'NONE',  ( 0.000000000000000000, 0.000000000000000000, 1.000000000000000000 ) ) ;
#3531 = EDGE_CURVE ( 'NONE', #2015, #20188, #12586, .T. ) ;
#3532 = ORIENTED_EDGE ( 'NONE', *, *, #16392, .F. ) ;
#3533 = DIRECTION ( 'NONE',  ( -1.000000000000000000, 0.000000000000000000, 0.000000000000000000 ) ) ;
#3534 = AXIS2_PLACEMENT_3D ( 'NONE', #21241, #17677, #19191 ) ;
#3535 = CIRCLE ( 'NONE', #6816, 17.00000000000000000 ) ;
#3536 = CIRCLE ( 'NONE', #6456, 2.099999999999997868 ) ;
#3537 = EDGE_CURVE ( 'NONE', #7411, #10689, #12893, .T. ) ;
#3538 = CARTESIAN_POINT ( 'NONE',  ( -27.84804035626028806, 24.75236754129139882, 2.999999999999995559 ) ) ;
#3539 = FACE_OUTER_BOUND ( 'NONE', #11919, .T. ) ;
#3540 = DIRECTION ( 'NONE',  ( 0.000000000000000000, -1.000000000000000000, 0.000000000000000000 ) ) ;
#3541 = ORIENTED_EDGE ( 'NONE', *, *, #7207, .F. ) ;
#3542 = CIRCLE ( 'NONE', #1701, 2.499999999999998668 ) ;
#3543 = ORIENTED_EDGE ( 'NONE', *, *, #22437, .F. ) ;
#3544 = ORIENTED_EDGE ( 'NONE', *, *, #21402, .F. ) ;
#3545 = CARTESIAN_POINT ( 'NONE',  ( -0.6864184775308176389, -1.216838870806101092, -47.75834167804065800 ) ) ;
#3546 = CARTESIAN_POINT ( 'NONE',  ( 11.85142133643347506, 39.99999999999999289, -54.27688992489011355 ) ) ;
#3547 = AXIS2_PLACEMENT_3D ( 'NONE', #20995, #19393, #1962 ) ;
#3548 = VERTEX_POINT ( 'NONE', #14420 ) ;
#3549 = DIRECTION ( 'NONE',  ( -6.505213034913038160E-19, -3.903127820947822896E-18, -1.000000000000000000 ) ) ;
#3550 = CARTESIAN_POINT ( 'NONE',  ( 7.310544252644470693E-15, 28.19616000222403684, 0.000000000000000000 ) ) ;
#3551 = CYLINDRICAL_SURFACE ( 'NONE', #287, 6.499999999999999112 ) ;
#3552 = EDGE_CURVE ( 'NONE', #7430, #16727, #3048, .T. ) ;
#3553 = CARTESIAN_POINT ( 'NONE',  ( -9.814839119317305460, 37.44644195123124319, -57.08682537453712769 ) ) ;
#3554 = DIRECTION ( 'NONE',  ( 0.1421319796954317316, 0.000000000000000000, -0.9898477157360405787 ) ) ;
#3555 = AXIS2_PLACEMENT_3D ( 'NONE', #21855, #6153, #16567 ) ;
#3556 = VERTEX_POINT ( 'NONE', #574 ) ;
#3557 = DIRECTION ( 'NONE',  ( -6.505213034913038160E-19, -3.903127820947822896E-18, -1.000000000000000000 ) ) ;
#3558 = FILL_AREA_STYLE ('',( #6642 ) ) ;
#3559 = DIRECTION ( 'NONE',  ( 0.000000000000000000, -1.000000000000000000, 0.000000000000000000 ) ) ;
#3560 = CARTESIAN_POINT ( 'NONE',  ( 34.99999999999980815, 28.00000000000000000, 52.49999999999922551 ) ) ;
#3561 = EDGE_CURVE ( 'NONE', #349, #8848, #15819, .T. ) ;
#3562 = ORIENTED_EDGE ( 'NONE', *, *, #11829, .F. ) ;
#3563 = DIRECTION ( 'NONE',  ( 0.000000000000000000, 1.000000000000000000, 0.000000000000000000 ) ) ;
#3564 = ORIENTED_EDGE ( 'NONE', *, *, #7437, .T. ) ;
#3565 = EDGE_CURVE ( 'NONE', #20227, #17027, #10702, .T. ) ;
#3566 = ORIENTED_EDGE ( 'NONE', *, *, #15790, .F. ) ;
#3567 = CARTESIAN_POINT ( 'NONE',  ( 2.602085213965210642E-15, -0.9047447100419790944, 0.000000000000000000 ) ) ;
#3568 = CARTESIAN_POINT ( 'NONE',  ( 0.2227364088704490985, -1.232651810762517064, 48.42315971483671433 ) ) ;
#3569 = CIRCLE ( 'NONE', #16363, 19.11328065563152379 ) ;
#3570 = DIRECTION ( 'NONE',  ( 0.000000000000000000, 1.000000000000000000, 0.000000000000000000 ) ) ;
#3571 = DIRECTION ( 'NONE',  ( -0.000000000000000000, -1.000000000000000000, -0.000000000000000000 ) ) ;
#3572 = CARTESIAN_POINT ( 'NONE',  ( -15.49999999999980460, -2.516660498395515866, 100.0000000000000000 ) ) ;
#3573 = VECTOR ( 'NONE', #18015, 1000.000000000000000 ) ;
#3574 = ORIENTED_EDGE ( 'NONE', *, *, #14203, .F. ) ;
#3575 = LINE ( 'NONE', #8602, #7278 ) ;
#3576 = CARTESIAN_POINT ( 'NONE',  ( -26.10603996529605553, -24.10117729468409209, 3.000000000000057732 ) ) ;
#3577 = ORIENTED_EDGE ( 'NONE', *, *, #8483, .F. ) ;
#3578 = ADVANCED_FACE ( 'NONE', ( #7679 ), #21660, .T. ) ;
#3579 = CYLINDRICAL_SURFACE ( 'NONE', #8684, 2.499999999999995115 ) ;
#3580 = AXIS2_PLACEMENT_3D ( 'NONE', #16373, #5950, #19932 ) ;
#3581 = DIRECTION ( 'NONE',  ( 0.000000000000000000, 1.000000000000000000, 0.000000000000000000 ) ) ;
#3582 = CARTESIAN_POINT ( 'NONE',  ( 24.62019382530525391, -4.341204441673101933, -2.999999999999999112 ) ) ;
#3583 = LINE ( 'NONE', #7883, #7896 ) ;
#3584 = CYLINDRICAL_SURFACE ( 'NONE', #17715, 20.00000000000000000 ) ;
#3585 = ORIENTED_EDGE ( 'NONE', *, *, #21827, .F. ) ;
#3586 = DIRECTION ( 'NONE',  ( -1.000000000000000000, 0.000000000000000000, 0.000000000000000000 ) ) ;
#3587 = DIRECTION ( 'NONE',  ( -6.505213034913038160E-19, -3.903127820947822896E-18, -1.000000000000000000 ) ) ;
#3588 = CARTESIAN_POINT ( 'NONE',  ( -17.98964431006460174, 6.536084871031949461, 57.54127157382312419 ) ) ;
#3589 = EDGE_LOOP ( 'NONE', ( #3395, #17004 ) ) ;
#3590 = CARTESIAN_POINT ( 'NONE',  ( 13.56354382738799735, 2.142135623730926142, 56.03997097393686033 ) ) ;
#3591 = CIRCLE ( 'NONE', #9793, 19.11328065563152379 ) ;
#3592 = CIRCLE ( 'NONE', #12346, 5.000000000000000000 ) ;
#3593 = FACE_OUTER_BOUND ( 'NONE', #1491, .T. ) ;
#3594 = EDGE_CURVE ( 'NONE', #2221, #3795, #10326, .T. ) ;
#3595 = CYLINDRICAL_SURFACE ( 'NONE', #14729, 2.499999999999995115 ) ;
#3596 = B_SPLINE_CURVE_WITH_KNOTS ( 'NONE', 3,
 ( #19002, #9713, #10604, #10269, #8675, #8560, #7175, #5143, #15533, #19223, #14144, #7063, #22557, #1571, #9008, #6853, #12331, #17493, #8794, #10375, #13817, #20835 ),
 .UNSPECIFIED., .F., .F.,
 ( 4, 2, 2, 2, 2, 2, 2, 2, 2, 2, 4 ),
 ( 0.000000000000000000, 0.005822207826702250309, 0.007277759783377815705, 0.008733311740053380234, 0.01164441565340452317, 0.01309996761008009464, 0.01455551956675566784, 0.01746662348010682292, 0.01892217543678240133, 0.02037772739345797973, 0.02328883130680912961 ),
 .UNSPECIFIED. ) ;
#3597 = AXIS2_PLACEMENT_3D ( 'NONE', #1510, #21098, #5291 ) ;
#3598 = VECTOR ( 'NONE', #7421, 1000.000000000000000 ) ;
#3599 = ADVANCED_FACE ( 'NONE', ( #4366 ), #13245, .T. ) ;
#3600 = EDGE_LOOP ( 'NONE', ( #715, #15242 ) ) ;
#3601 = EDGE_LOOP ( 'NONE', ( #21781, #13201, #16226, #1209 ) ) ;
#3602 = ADVANCED_FACE ( 'NONE', ( #16841 ), #20167, .F. ) ;
#3603 = ORIENTED_EDGE ( 'NONE', *, *, #2128, .F. ) ;
#3604 = VERTEX_POINT ( 'NONE', #13376 ) ;
#3605 = FACE_OUTER_BOUND ( 'NONE', #3141, .T. ) ;
#3606 = DIRECTION ( 'NONE',  ( -1.000000000000000000, 0.000000000000000000, 0.000000000000000000 ) ) ;
#3607 = CARTESIAN_POINT ( 'NONE',  ( 27.62019382530527878, -4.341204441673157888, 3.000000000000023537 ) ) ;
#3608 = CARTESIAN_POINT ( 'NONE',  ( 7.474202570536298218, -30.60042966911724704, 2.999999999999995559 ) ) ;
#3609 = VECTOR ( 'NONE', #18766, 1000.000000000000000 ) ;
#3610 = ORIENTED_EDGE ( 'NONE', *, *, #97, .T. ) ;
#3611 = CARTESIAN_POINT ( 'NONE',  ( 30.13956425491254265, 21.05198877411773495, 2.800654218530485018 ) ) ;
#3612 = DIRECTION ( 'NONE',  ( 1.296372316667914327E-16, 1.000000000000000000, -0.000000000000000000 ) ) ;
#3613 = ORIENTED_EDGE ( 'NONE', *, *, #19693, .T. ) ;
#3614 = CARTESIAN_POINT ( 'NONE',  ( -13.32368996328071376, 38.03919112700260285, -55.94897837928603934 ) ) ;
#3615 = VECTOR ( 'NONE', #10576, 1000.000000000000000 ) ;
#3616 = ORIENTED_EDGE ( 'NONE', *, *, #3163, .F. ) ;
#3617 = CARTESIAN_POINT ( 'NONE',  ( 0.5350771668691457483, 35.00000000000000711, 38.73397172404481381 ) ) ;
#3618 = ORIENTED_EDGE ( 'NONE', *, *, #2825, .T. ) ;
#3619 = CARTESIAN_POINT ( 'NONE',  ( 0.7832304697071968969, 40.00000000000098055, -49.34583672932542697 ) ) ;
#3620 = CARTESIAN_POINT ( 'NONE',  ( -1.387778780781445676E-14, 20.00000000000000000, 101.0000000000000568 ) ) ;
#3621 = CONICAL_SURFACE ( 'NONE', #5416, 2.524999999999999467, 0.7853981633974482790 ) ;
#3622 = CARTESIAN_POINT ( 'NONE',  ( 13.00000000000024336, -2.516660498395250745, 105.0000000000000142 ) ) ;
#3623 = EDGE_CURVE ( 'NONE', #22687, #9796, #7787, .T. ) ;
#3624 = CARTESIAN_POINT ( 'NONE',  ( 19.80330599461103702, 22.93419722094642310, 60.57506235960030239 ) ) ;
#3625 = FACE_BOUND ( 'NONE', #8762, .T. ) ;
#3626 = DIRECTION ( 'NONE',  ( 0.000000000000000000, -1.000000000000000000, 0.000000000000000000 ) ) ;
#3627 = CIRCLE ( 'NONE', #7999, 1.000000000000000888 ) ;
#3628 = AXIS2_PLACEMENT_3D ( 'NONE', #20536, #22486, #17081 ) ;
#3629 = ORIENTED_EDGE ( 'NONE', *, *, #13058, .F. ) ;
#3630 = AXIS2_PLACEMENT_3D ( 'NONE', #10820, #12875, #6021 ) ;
#3631 = AXIS2_PLACEMENT_3D ( 'NONE', #16764, #9658, #8064 ) ;
#3632 = ORIENTED_EDGE ( 'NONE', *, *, #16597, .F. ) ;
#3633 = ORIENTED_EDGE ( 'NONE', *, *, #2637, .T. ) ;
#3634 = AXIS2_PLACEMENT_3D ( 'NONE', #3461, #20534, #4836 ) ;
#3635 = VERTEX_POINT ( 'NONE', #11450 ) ;
#3636 = DIRECTION ( 'NONE',  ( 1.000000000000000000, 1.208970125616063490E-17, 0.000000000000000000 ) ) ;
#3637 = CARTESIAN_POINT ( 'NONE',  ( -34.99999999999980815, 40.00000000000000711, 57.52499999999922409 ) ) ;
#3638 = CARTESIAN_POINT ( 'NONE',  ( -9.999999999999980460, -3.000000000000002665, 4.999999999999997335 ) ) ;
#3639 = FACE_OUTER_BOUND ( 'NONE', #22407, .T. ) ;
#3640 = CARTESIAN_POINT ( 'NONE',  ( 3.069013497901954324, 39.94370175202870854, 50.97148194424899970 ) ) ;
#3641 = AXIS2_PLACEMENT_3D ( 'NONE', #12545, #21617, #18050 ) ;
#3642 = EDGE_LOOP ( 'NONE', ( #15490, #98, #17559 ) ) ;
#3643 = CARTESIAN_POINT ( 'NONE',  ( 2.775557561562891351E-14, -2.775557561562891351E-14, 2.999999999999995559 ) ) ;
#3644 = CARTESIAN_POINT ( 'NONE',  ( -42.50000000000000711, -12.00000000000000000, -41.00000000000000000 ) ) ;
#3645 = VECTOR ( 'NONE', #10787, 1000.000000000000000 ) ;
#3646 = DIRECTION ( 'NONE',  ( -0.000000000000000000, -0.000000000000000000, 1.000000000000000000 ) ) ;
#3647 = CARTESIAN_POINT ( 'NONE',  ( 35.99819890246980236, -7.463862311151397755, -2.800654218530467698 ) ) ;
#3648 = FILL_AREA_STYLE ('',( #2506 ) ) ;
#3649 = EDGE_CURVE ( 'NONE', #22210, #15922, #4122, .T. ) ;
#3650 = FACE_OUTER_BOUND ( 'NONE', #16599, .T. ) ;
#3651 = CARTESIAN_POINT ( 'NONE',  ( -6.869664380963927286, 39.72569445733122961, 53.24677099177210948 ) ) ;
#3652 = EDGE_CURVE ( 'NONE', #11550, #1500, #6318, .T. ) ;
#3653 = CARTESIAN_POINT ( 'NONE',  ( -42.49999999999996447, 10.00000000000000000, -50.00000000000000711 ) ) ;
#3654 = DIRECTION ( 'NONE',  ( 0.000000000000000000, 0.000000000000000000, -1.000000000000000000 ) ) ;
#3655 = ORIENTED_EDGE ( 'NONE', *, *, #10356, .F. ) ;
#3656 = ORIENTED_EDGE ( 'NONE', *, *, #4032, .T. ) ;
#3657 = CIRCLE ( 'NONE', #5117, 2.499999999999995115 ) ;
#3658 = EDGE_CURVE ( 'NONE', #20269, #105, #12927, .T. ) ;
#3659 = ORIENTED_EDGE ( 'NONE', *, *, #266, .T. ) ;
#3660 = DIRECTION ( 'NONE',  ( -1.000000000000000000, -1.208970125616046080E-17, 6.505213034913038160E-19 ) ) ;
#3661 = DIRECTION ( 'NONE',  ( 0.000000000000000000, 0.000000000000000000, -1.000000000000000000 ) ) ;
#3662 = EDGE_CURVE ( 'NONE', #2563, #10262, #11070, .T. ) ;
#3663 = CARTESIAN_POINT ( 'NONE',  ( 15.99999999999991651, 20.00000000000000000, 102.0000000000000142 ) ) ;
#3664 = FACE_OUTER_BOUND ( 'NONE', #2790, .T. ) ;
#3665 = CARTESIAN_POINT ( 'NONE',  ( 35.16985127952396084, 10.70799354677376414, 2.800654218530485018 ) ) ;
#3666 = CARTESIAN_POINT ( 'NONE',  ( 35.00000000000000000, 17.00000000000000000, -38.99999999999999289 ) ) ;
#3667 = CARTESIAN_POINT ( 'NONE',  ( 2.602085213965210642E-15, 0.6398376396478597794, 0.000000000000000000 ) ) ;
#3668 = VECTOR ( 'NONE', #2141, 1000.000000000000000 ) ;
#3669 = ORIENTED_EDGE ( 'NONE', *, *, #10893, .T. ) ;
#3670 = CARTESIAN_POINT ( 'NONE',  ( -10.49999999999980460, -2.516660498395516310, 100.0000000000000000 ) ) ;
#3671 = DIRECTION ( 'NONE',  ( 1.296372316667914327E-16, 1.000000000000000000, -0.000000000000000000 ) ) ;
#3672 =( LENGTH_UNIT ( ) NAMED_UNIT ( * ) SI_UNIT ( .MILLI., .METRE. ) );
#3673 = DIRECTION ( 'NONE',  ( -0.000000000000000000, 1.000000000000000000, -0.000000000000000000 ) ) ;
#3674 = DIRECTION ( 'NONE',  ( 0.000000000000000000, 0.000000000000000000, -1.000000000000000000 ) ) ;
#3675 = EDGE_LOOP ( 'NONE', ( #17661, #14381, #14341 ) ) ;
#3676 = DIRECTION ( 'NONE',  ( 0.000000000000000000, 0.000000000000000000, -1.000000000000000000 ) ) ;
#3677 = DIRECTION ( 'NONE',  ( 0.000000000000000000, 0.000000000000000000, -1.000000000000000000 ) ) ;
#3678 = AXIS2_PLACEMENT_3D ( 'NONE', #19935, #8024, #14982 ) ;
#3679 = VERTEX_POINT ( 'NONE', #18675 ) ;
#3680 = EDGE_CURVE ( 'NONE', #3268, #11125, #9240, .T. ) ;
#3681 = ITEM_DEFINED_TRANSFORMATION ( 'NONE', 'NONE', #2546,  #18273 ) ;
#3682 = ORIENTED_EDGE ( 'NONE', *, *, #15109, .T. ) ;
#3683 = CARTESIAN_POINT ( 'NONE',  ( -2.673152730111970410, 23.56975547524771741, 6.612623190900161596 ) ) ;
#3684 = EDGE_CURVE ( 'NONE', #1286, #9683, #16381, .T. ) ;
#3685 = FACE_OUTER_BOUND ( 'NONE', #22154, .T. ) ;
#3686 = DIRECTION ( 'NONE',  ( -0.000000000000000000, 1.000000000000000000, -0.000000000000000000 ) ) ;
#3687 = CARTESIAN_POINT ( 'NONE',  ( -14.74639653023226948, 28.96193690644935259, 2.999999999999995559 ) ) ;
#3688 = VERTEX_POINT ( 'NONE', #696 ) ;
#3689 = DIRECTION ( 'NONE',  ( 6.505213034913038160E-19, 3.903127820947822896E-18, 1.000000000000000000 ) ) ;
#3690 = DIRECTION ( 'NONE',  ( -1.000000000000000000, -5.863186540146433761E-14, 0.000000000000000000 ) ) ;
#3691 = ORIENTED_EDGE ( 'NONE', *, *, #22016, .F. ) ;
#3692 = CARTESIAN_POINT ( 'NONE',  ( 0.000000000000000000, 30.00000000000000000, 0.000000000000000000 ) ) ;
#3693 = CARTESIAN_POINT ( 'NONE',  ( -24.24871130596435620, 13.99999999999990052, 2.999999999999995559 ) ) ;
#3695 = TOROIDAL_SURFACE ( 'NONE', #7328, 34.90673715956759082, 8.750000000000000000 ) ;
#3694 = CARTESIAN_POINT ( 'NONE',  ( -41.39271818392631985, 7.000000000000000000, 5.943569790512528428 ) ) ;
#3696 = DIRECTION ( 'NONE',  ( -1.000000000000000000, 0.000000000000000000, 0.000000000000000000 ) ) ;
#3697 = ORIENTED_EDGE ( 'NONE', *, *, #21032, .T. ) ;
#3698 = DIRECTION ( 'NONE',  ( 0.000000000000000000, 0.000000000000000000, 1.000000000000000000 ) ) ;
#3699 = LINE ( 'NONE', #3045, #10172 ) ;
#3700 = CARTESIAN_POINT ( 'NONE',  ( -2.098978802144722877, 39.97352552835178585, -50.29629877501648849 ) ) ;
#3701 = ORIENTED_EDGE ( 'NONE', *, *, #14762, .T. ) ;
#3702 = ADVANCED_FACE ( 'NONE', ( #802 ), #13255, .F. ) ;
#3703 = DIRECTION ( 'NONE',  ( 6.505213034913038160E-19, 3.903127820947822896E-18, 1.000000000000000000 ) ) ;
#3704 = CARTESIAN_POINT ( 'NONE',  ( -35.00000000000058265, 40.00000000000000711, -57.52500000000076597 ) ) ;
#3705 = EDGE_CURVE ( 'NONE', #7282, #7391, #83, .T. ) ;
#3706 = ORIENTED_EDGE ( 'NONE', *, *, #4297, .T. ) ;
#3707 = AXIS2_PLACEMENT_3D ( 'NONE', #7589, #19856, #6215 ) ;
#3708 = ORIENTED_EDGE ( 'NONE', *, *, #13091, .T. ) ;
#3709 = ORIENTED_EDGE ( 'NONE', *, *, #14294, .F. ) ;
#3710 = ORIENTED_EDGE ( 'NONE', *, *, #20129, .T. ) ;
#3711 = DIRECTION ( 'NONE',  ( 0.000000000000000000, 0.000000000000000000, 1.000000000000000000 ) ) ;
#3712 = CARTESIAN_POINT ( 'NONE',  ( 5.551115123125782702E-14, -1.387778780781445676E-13, -5.749999999999949374 ) ) ;
#3713 = CARTESIAN_POINT ( 'NONE',  ( 4.995691471223772773, 39.84469977656465289, -52.21048576823625353 ) ) ;
#3714 = CARTESIAN_POINT ( 'NONE',  ( 1.679961057847793704, 39.99999999999999289, 49.78369069256650192 ) ) ;
#3715 = VERTEX_POINT ( 'NONE', #18327 ) ;
#3716 = CARTESIAN_POINT ( 'NONE',  ( 3.330669073875469621E-13, -1.110223024625156540E-13, -2.999999999999971578 ) ) ;
#3717 = DIRECTION ( 'NONE',  ( -0.000000000000000000, 1.000000000000000000, -0.000000000000000000 ) ) ;
#3718 = ORIENTED_EDGE ( 'NONE', *, *, #17841, .T. ) ;
#3719 = CARTESIAN_POINT ( 'NONE',  ( -31.11359284679371484, -4.918774254216190300, -7.000000000000006217 ) ) ;
#3720 = CARTESIAN_POINT ( 'NONE',  ( -18.83430946916727322, 32.25183488571026658, -57.78319592314316822 ) ) ;
#3721 = DIRECTION ( 'NONE',  ( -6.505213034913038160E-19, -3.903127820947822896E-18, -1.000000000000000000 ) ) ;
#3722 = VERTEX_POINT ( 'NONE', #2644 ) ;
#3723 = DIRECTION ( 'NONE',  ( 0.000000000000000000, 0.000000000000000000, -1.000000000000000000 ) ) ;
#3724 = ORIENTED_EDGE ( 'NONE', *, *, #1340, .F. ) ;
#3725 = FACE_OUTER_BOUND ( 'NONE', #8858, .T. ) ;
#3726 = CARTESIAN_POINT ( 'NONE',  ( -0.6233897118003940419, 39.99089506582289744, 49.47139888151596665 ) ) ;
#3727 = CARTESIAN_POINT ( 'NONE',  ( 15.00354810072215095, -32.89319786336249507, -2.933296326616342764 ) ) ;
#3728 = EDGE_CURVE ( 'NONE', #4117, #15875, #11441, .T. ) ;
#3729 = CARTESIAN_POINT ( 'NONE',  ( 19.65511384563453490, 23.80142929986463329, 60.53962097676932075 ) ) ;
#3730 = CARTESIAN_POINT ( 'NONE',  ( -34.99999999999999289, -3.999999999999985345, -3.012171160963566127E-14 ) ) ;
#3731 = CARTESIAN_POINT ( 'NONE',  ( 13.85640646055130709, 1.500000000000004885, -4.000000000000099476 ) ) ;
#3732 = EDGE_CURVE ( 'NONE', #8574, #9457, #11569, .T. ) ;
#3733 = ADVANCED_FACE ( 'NONE', ( #3086 ), #20959, .F. ) ;
#3735 = ADVANCED_FACE ( 'NONE', ( #1246 ), #8465, .F. ) ;
#3734 = VERTEX_POINT ( 'NONE', #13488 ) ;
#3736 = VECTOR ( 'NONE', #15493, 1000.000000000000000 ) ;
#3737 = EDGE_LOOP ( 'NONE', ( #6138, #7809 ) ) ;
#3738 = ORIENTED_EDGE ( 'NONE', *, *, #21735, .F. ) ;
#3739 = ORIENTED_EDGE ( 'NONE', *, *, #7664, .T. ) ;
#3740 = DIRECTION ( 'NONE',  ( 0.000000000000000000, 0.000000000000000000, -1.000000000000000000 ) ) ;
#3741 = CARTESIAN_POINT ( 'NONE',  ( 5.999999999999999112, -40.00000000000000000, -6.000000000000000000 ) ) ;
#3742 = CARTESIAN_POINT ( 'NONE',  ( -34.99999999999997868, 0.000000000000000000, 54.99999999999698730 ) ) ;
#3743 = EDGE_CURVE ( 'NONE', #14737, #4123, #16934, .T. ) ;
#3744 = LINE ( 'NONE', #9429, #22652 ) ;
#3745 = CARTESIAN_POINT ( 'NONE',  ( 0.01154789369496759741, 39.99999926358022861, 48.74295989195564971 ) ) ;
#3746 = ORIENTED_EDGE ( 'NONE', *, *, #11418, .T. ) ;
#3747 = CARTESIAN_POINT ( 'NONE',  ( 9.857944917841363619, 0.2919354798322448263, -54.29891737064843937 ) ) ;
#3748 = CARTESIAN_POINT ( 'NONE',  ( 32.28023859650885186, 14.85562396683469544, -2.999999999999997780 ) ) ;
#3749 = DIRECTION ( 'NONE',  ( 0.000000000000000000, 1.000000000000000000, 0.000000000000000000 ) ) ;
#3750 = DIRECTION ( 'NONE',  ( 0.000000000000000000, -1.000000000000000000, 0.000000000000000000 ) ) ;
#3751 = CARTESIAN_POINT ( 'NONE',  ( -8.916870955515580732, 2.080241304161461358, -56.50845996868350340 ) ) ;
#3752 =( REPRESENTATION_RELATIONSHIP ('NONE','NONE', #8442, #18960 ) REPRESENTATION_RELATIONSHIP_WITH_TRANSFORMATION ( #20974 )SHAPE_REPRESENTATION_RELATIONSHIP( ) );
#3753 = CIRCLE ( 'NONE', #16546, 34.90673715956759082 ) ;
#3754 = CARTESIAN_POINT ( 'NONE',  ( -42.49999999999996447, 7.000000000000000000, -47.50000000000000711 ) ) ;
#3755 = DIRECTION ( 'NONE',  ( -6.505213034913038160E-19, -3.903127820947822896E-18, -1.000000000000000000 ) ) ;
#3756 = CARTESIAN_POINT ( 'NONE',  ( 3.849727973822421485E-15, 1.499999999999997780, 0.000000000000000000 ) ) ;
#3757 = EDGE_LOOP ( 'NONE', ( #17591, #3051, #11838, #12422 ) ) ;
#3758 = EDGE_LOOP ( 'NONE', ( #16747, #22171, #10337, #18642 ) ) ;
#3759 = EDGE_CURVE ( 'NONE', #3823, #19682, #22455, .T. ) ;
#3760 = VERTEX_POINT ( 'NONE', #17389 ) ;
#3761 = LINE ( 'NONE', #314, #16607 ) ;
#3762 = CONICAL_SURFACE ( 'NONE', #2281, 2.099999999999997868, 1.029744258676653867 ) ;
#3763 = EDGE_CURVE ( 'NONE', #2693, #10299, #3327, .T. ) ;
#3764 = CARTESIAN_POINT ( 'NONE',  ( 11.12223430625389753, 40.00000000000000000, -54.01173000072967056 ) ) ;
#3765 = CIRCLE ( 'NONE', #18773, 25.00000000000000000 ) ;
#3766 = DIRECTION ( 'NONE',  ( -6.505213034913038160E-19, -3.903127820947822896E-18, -1.000000000000000000 ) ) ;
#3767 = EDGE_CURVE ( 'NONE', #21906, #4376, #1710, .T. ) ;
#3768 = FACE_OUTER_BOUND ( 'NONE', #9363, .T. ) ;
#3769 = CARTESIAN_POINT ( 'NONE',  ( -20.00000000000001421, 20.00000000000000355, 60.62177826491070931 ) ) ;
#3770 = CARTESIAN_POINT ( 'NONE',  ( -10.50000000000012079, 42.51666049839536043, -105.0010000000000048 ) ) ;
#3771 = DIRECTION ( 'NONE',  ( 0.9659258262890680902, -0.2588190451025210170, 0.000000000000000000 ) ) ;
#3772 = ORIENTED_EDGE ( 'NONE', *, *, #9384, .T. ) ;
#3773 = CARTESIAN_POINT ( 'NONE',  ( -20.00000000000001421, 20.00000000000000355, 98.00000000000000000 ) ) ;
#3774 = CARTESIAN_POINT ( 'NONE',  ( -35.00000000000058265, 28.00000000000000000, -55.00000000000076028 ) ) ;
#3775 = CARTESIAN_POINT ( 'NONE',  ( 35.00000000000000000, 0.000000000000000000, 4.258610482196280173E-15 ) ) ;
#3776 = AXIS2_PLACEMENT_3D ( 'NONE', #15912, #7336, #230 ) ;
#3777 = ORIENTED_EDGE ( 'NONE', *, *, #7700, .F. ) ;
#3778 = CARTESIAN_POINT ( 'NONE',  ( 12.00000000000000355, 1.500000000000003553, 0.000000000000000000 ) ) ;
#3779 = DIRECTION ( 'NONE',  ( -1.000000000000000000, -7.986889777657331544E-15, 0.000000000000000000 ) ) ;
#3780 = VECTOR ( 'NONE', #5970, 1000.000000000000000 ) ;
#3781 = CARTESIAN_POINT ( 'NONE',  ( 14.69246073108732631, 6.394048232432887779, -56.48929660089486049 ) ) ;
#3782 = EDGE_CURVE ( 'NONE', #9695, #9796, #15672, .T. ) ;
#3783 = ORIENTED_EDGE ( 'NONE', *, *, #22592, .T. ) ;
#3784 = CONTEXT_DEPENDENT_SHAPE_REPRESENTATION ( #16620, #6206 ) ;
#3785 = EDGE_LOOP ( 'NONE', ( #20669, #19567, #10195, #9967 ) ) ;
#3786 = CARTESIAN_POINT ( 'NONE',  ( 0.09368790929011092117, 39.99996055670441564, -48.80680027770784335 ) ) ;
#3787 = DIRECTION ( 'NONE',  ( -6.505213034913038160E-19, -3.903127820947822896E-18, -1.000000000000000000 ) ) ;
#3788 = AXIS2_PLACEMENT_3D ( 'NONE', #4224, #7886, #20151 ) ;
#3789 = DIRECTION ( 'NONE',  ( 0.000000000000000000, 1.000000000000000000, 0.000000000000000000 ) ) ;
#3790 = DIRECTION ( 'NONE',  ( 0.000000000000000000, 0.000000000000000000, 1.000000000000000000 ) ) ;
#3791 = VERTEX_POINT ( 'NONE', #8576 ) ;
#3792 = DIRECTION ( 'NONE',  ( -1.000000000000000000, -1.208970125616044077E-17, 0.000000000000000000 ) ) ;
#3793 = AXIS2_PLACEMENT_3D ( 'NONE', #3218, #6646, #4821 ) ;
#3794 = CARTESIAN_POINT ( 'NONE',  ( -7.531924820109092700, 39.99999999999999289, 52.77310267448202552 ) ) ;
#3795 = VERTEX_POINT ( 'NONE', #20853 ) ;
#3796 = DIRECTION ( 'NONE',  ( 6.505213034913038160E-19, 3.903127820947822896E-18, 1.000000000000000000 ) ) ;
#3797 = CIRCLE ( 'NONE', #16596, 2.500000000000002220 ) ;
#3798 = CARTESIAN_POINT ( 'NONE',  ( 22.32664865868312276, 17.89874346835044960, -58.64628984943159651 ) ) ;
#3799 = CARTESIAN_POINT ( 'NONE',  ( -1.387778780781445518E-14, 20.00000000000000355, 102.0000000000000142 ) ) ;
#3800 = ORIENTED_EDGE ( 'NONE', *, *, #4187, .T. ) ;
#3801 = LINE ( 'NONE', #15709, #15952 ) ;
#3802 = CARTESIAN_POINT ( 'NONE',  ( -11.68090480754625027, 3.765577839755239076, 57.90797000640172598 ) ) ;
#3803 = CARTESIAN_POINT ( 'NONE',  ( -4.585174533585286483, 39.86909732232018655, -51.95486270304797216 ) ) ;
#3804 = ADVANCED_FACE ( 'NONE', ( #15549 ), #9950, .T. ) ;
#3805 = ORIENTED_EDGE ( 'NONE', *, *, #7613, .F. ) ;
#3806 = CARTESIAN_POINT ( 'NONE',  ( 2.220446049250313081E-13, 2.775557561562891351E-14, -2.800654218530485018 ) ) ;
#3807 = CARTESIAN_POINT ( 'NONE',  ( 34.24928931925771991, -6.742883674876576805, -2.999999999999971578 ) ) ;
#3808 = EDGE_CURVE ( 'NONE', #8847, #16743, #12022, .T. ) ;
#3809 = EDGE_CURVE ( 'NONE', #7645, #10705, #191, .T. ) ;
#3810 = EDGE_CURVE ( 'NONE', #6428, #19994, #12129, .T. ) ;
#3811 = CIRCLE ( 'NONE', #21753, 2.499999999999995115 ) ;
#3812 = MECHANICAL_DESIGN_GEOMETRIC_PRESENTATION_REPRESENTATION (  '', ( #13668 ), #11862 ) ;
#3813 = ORIENTED_EDGE ( 'NONE', *, *, #19503, .T. ) ;
#3814 = ORIENTED_EDGE ( 'NONE', *, *, #14239, .F. ) ;
#3815 = EDGE_LOOP ( 'NONE', ( #2074, #13522, #4848, #12384 ) ) ;
#3816 = ORIENTED_EDGE ( 'NONE', *, *, #21685, .T. ) ;
#3817 = CARTESIAN_POINT ( 'NONE',  ( -42.50000000000000711, -12.00000000000012434, 50.02500000000011937 ) ) ;
#3818 = FACE_OUTER_BOUND ( 'NONE', #18240, .T. ) ;
#3819 = CARTESIAN_POINT ( 'NONE',  ( -30.13956425491219449, -21.05198877411826430, 2.800654218530505890 ) ) ;
#3820 = CARTESIAN_POINT ( 'NONE',  ( 9.952189117650823036, 40.00000000000000000, 53.64426396172073197 ) ) ;
#3821 = EDGE_CURVE ( 'NONE', #19682, #15823, #19125, .T. ) ;
#3822 = AXIS2_PLACEMENT_3D ( 'NONE', #16250, #17976, #6919 ) ;
#3823 = VERTEX_POINT ( 'NONE', #4920 ) ;
#3824 = LINE ( 'NONE', #4059, #3645 ) ;
#3825 = CARTESIAN_POINT ( 'NONE',  ( 10.39230484541348432, 1.500000000000003109, -6.000000000000073719 ) ) ;
#3826 = ORIENTED_EDGE ( 'NONE', *, *, #4433, .F. ) ;
#3827 = LINE ( 'NONE', #3942, #3573 ) ;
#3828 = CARTESIAN_POINT ( 'NONE',  ( -20.16756852208517259, 29.88972976525007397, -58.13897502025236719 ) ) ;
#3829 = CARTESIAN_POINT ( 'NONE',  ( -35.00000000000058265, 40.00000000000000000, -52.50000000000076739 ) ) ;
#3830 = VERTEX_POINT ( 'NONE', #11894 ) ;
#3831 = CARTESIAN_POINT ( 'NONE',  ( 0.000000000000000000, 29.97499999999999787, 0.000000000000000000 ) ) ;
#3832 = EDGE_LOOP ( 'NONE', ( #10837, #10650, #12585, #7543 ) ) ;
#3833 = CARTESIAN_POINT ( 'NONE',  ( 35.00000000000000000, 0.000000000000000000, 2.365113165210053967E-14 ) ) ;
#3834 = EDGE_CURVE ( 'NONE', #4643, #16803, #18900, .T. ) ;
#3835 = CARTESIAN_POINT ( 'NONE',  ( -16.66666666666665719, -20.00000000000000000, 23.57022603955159923 ) ) ;
#3836 = DIRECTION ( 'NONE',  ( -1.000000000000000000, 1.301042606982605814E-16, 0.000000000000000000 ) ) ;
#3837 = AXIS2_PLACEMENT_3D ( 'NONE', #8979, #3838, #7382 ) ;
#3838 = DIRECTION ( 'NONE',  ( 0.000000000000000000, 1.000000000000000000, 0.000000000000000000 ) ) ;
#3839 = CARTESIAN_POINT ( 'NONE',  ( 18.64599517736090917, 12.71385791664973652, 57.77541544179720745 ) ) ;
#3840 = FACE_OUTER_BOUND ( 'NONE', #12988, .T. ) ;
#3841 = EDGE_CURVE ( 'NONE', #12228, #4040, #14716, .T. ) ;
#3842 = CARTESIAN_POINT ( 'NONE',  ( 9.165377225651162973, 37.79989650906289711, -54.16098472236620864 ) ) ;
#3843 = ORIENTED_EDGE ( 'NONE', *, *, #8108, .F. ) ;
#3844 = CIRCLE ( 'NONE', #14432, 2.499999999999998668 ) ;
#3845 = VERTEX_POINT ( 'NONE', #4000 ) ;
#3846 = ORIENTED_EDGE ( 'NONE', *, *, #3162, .T. ) ;
#3847 = EDGE_LOOP ( 'NONE', ( #20703, #21022, #16887, #11706 ) ) ;
#3848 = DIRECTION ( 'NONE',  ( 1.000000000000000000, 0.000000000000000000, 0.000000000000000000 ) ) ;
#3849 = DIRECTION ( 'NONE',  ( 0.000000000000000000, 0.000000000000000000, 1.000000000000000000 ) ) ;
#3850 = DIRECTION ( 'NONE',  ( 0.000000000000000000, 0.000000000000000000, 1.000000000000000000 ) ) ;
#3851 = EDGE_CURVE ( 'NONE', #4605, #17185, #19492, .T. ) ;
#3852 = CARTESIAN_POINT ( 'NONE',  ( -32.09841355225981374, 5.093313992686310243, -7.000000000000006217 ) ) ;
#3853 = CARTESIAN_POINT ( 'NONE',  ( 0.3255751848036408935, 39.99938829199252410, 48.98576722398500038 ) ) ;
#3854 = CIRCLE ( 'NONE', #9697, 10.00000000000000178 ) ;
#3855 = CIRCLE ( 'NONE', #9702, 11.99999999999985256 ) ;
#3856 = ORIENTED_EDGE ( 'NONE', *, *, #14469, .F. ) ;
#3857 = DIRECTION ( 'NONE',  ( -1.000000000000000000, 0.000000000000000000, 0.000000000000000000 ) ) ;
#3858 = LINE ( 'NONE', #11145, #15632 ) ;
#3859 = DIRECTION ( 'NONE',  ( -1.000000000000000000, 1.084202172485504927E-16, 0.000000000000000000 ) ) ;
#3860 = EDGE_CURVE ( 'NONE', #17205, #20094, #321, .T. ) ;
#3861 = CARTESIAN_POINT ( 'NONE',  ( 2.220446049250313081E-13, 2.775557561562891351E-14, -2.800654218530485018 ) ) ;
#3862 = DIRECTION ( 'NONE',  ( -0.000000000000000000, -1.000000000000000000, -0.000000000000000000 ) ) ;
#3863 = AXIS2_PLACEMENT_3D ( 'NONE', #10380, #6970, #77 ) ;
#3864 = CARTESIAN_POINT ( 'NONE',  ( -24.99999999999999645, 20.00000000000000000, 25.00000000000001421 ) ) ;
#3865 = DIRECTION ( 'NONE',  ( 6.505213034913038160E-19, 3.903127820947822896E-18, 1.000000000000000000 ) ) ;
#3866 = DIRECTION ( 'NONE',  ( -6.505213034913038160E-19, -3.903127820947822896E-18, -1.000000000000000000 ) ) ;
#3867 = LINE ( 'NONE', #7409, #15598 ) ;
#3868 = EDGE_CURVE ( 'NONE', #15849, #12848, #19698, .T. ) ;
#3869 = CIRCLE ( 'NONE', #8977, 34.90673715956759082 ) ;
#3870 = VERTEX_POINT ( 'NONE', #17513 ) ;
#3871 = EDGE_CURVE ( 'NONE', #1691, #6084, #197, .T. ) ;
#3872 = CIRCLE ( 'NONE', #17395, 7.500000000000000000 ) ;
#3873 = VERTEX_POINT ( 'NONE', #1826 ) ;
#3874 = EDGE_CURVE ( 'NONE', #10976, #13471, #18753, .T. ) ;
#3875 = AXIS2_PLACEMENT_3D ( 'NONE', #16531, #16874, #2678 ) ;
#3876 = ORIENTED_EDGE ( 'NONE', *, *, #15734, .F. ) ;
#3877 = AXIS2_PLACEMENT_3D ( 'NONE', #5239, #3185, #19221 ) ;
#3878 = CARTESIAN_POINT ( 'NONE',  ( 42.50000000000000711, -12.00000000000000000, 45.40000000000001279 ) ) ;
#3879 = EDGE_CURVE ( 'NONE', #15473, #8378, #15446, .T. ) ;
#3880 = DIRECTION ( 'NONE',  ( -0.000000000000000000, 1.000000000000000000, -0.000000000000000000 ) ) ;
#3881 = CARTESIAN_POINT ( 'NONE',  ( 3.469446951953614189E-15, 6.776263578034402713E-17, 0.000000000000000000 ) ) ;
#3882 = DIRECTION ( 'NONE',  ( 0.7752116086454778898, 0.5577761202038522548, 0.2965345874457622211 ) ) ;
#3883 = CARTESIAN_POINT ( 'NONE',  ( -12.30135915900901011, 4.212003844039742262, 58.16904039079302180 ) ) ;
#3884 = CIRCLE ( 'NONE', #6453, 10.00000000000000178 ) ;
#3885 = CARTESIAN_POINT ( 'NONE',  ( -12.72045107882562220, 38.45933137995365314, -55.71167848415556278 ) ) ;
#3886 = VECTOR ( 'NONE', #22409, 1000.000000000000000 ) ;
#3887 = FACE_OUTER_BOUND ( 'NONE', #18134, .T. ) ;
#3888 = AXIS2_PLACEMENT_3D ( 'NONE', #9576, #4321, #7743 ) ;
#3889 = ORIENTED_EDGE ( 'NONE', *, *, #2659, .F. ) ;
#3890 = FACE_BOUND ( 'NONE', #11880, .T. ) ;
#3891 = CARTESIAN_POINT ( 'NONE',  ( -10.00000000000000000, -4.824555320336763486, -3.000000000000000000 ) ) ;
#3892 = CARTESIAN_POINT ( 'NONE',  ( 12.68897045256291811, 11.99170770793163321, -44.74667050109238176 ) ) ;
#3893 = EDGE_CURVE ( 'NONE', #19116, #6177, #17051, .T. ) ;
#3894 = AXIS2_PLACEMENT_3D ( 'NONE', #11883, #13478, #13700 ) ;
#3895 = EDGE_LOOP ( 'NONE', ( #5883, #8008, #16558, #2914 ) ) ;
#3896 = ADVANCED_FACE ( 'NONE', ( #5370 ), #7177, .T. ) ;
#3897 = DIRECTION ( 'NONE',  ( -0.000000000000000000, 1.000000000000000000, -0.000000000000000000 ) ) ;
#3898 = CARTESIAN_POINT ( 'NONE',  ( 35.00000000000000000, 40.00000000000000000, 4.258610482196280173E-15 ) ) ;
#3899 = CARTESIAN_POINT ( 'NONE',  ( -20.54749497201914465, 29.74882400976386521, 2.932969818539061801 ) ) ;
#3900 = ADVANCED_FACE ( 'NONE', ( #21293 ), #8809, .T. ) ;
#3901 = AXIS2_PLACEMENT_3D ( 'NONE', #297, #14690, #5237 ) ;
#3902 = ORIENTED_EDGE ( 'NONE', *, *, #12487, .F. ) ;
#3903 = VECTOR ( 'NONE', #1289, 1000.000000000000000 ) ;
#3904 = AXIS2_PLACEMENT_3D ( 'NONE', #2334, #21939, #12752 ) ;
#3905 = VERTEX_POINT ( 'NONE', #15887 ) ;
#3906 = CONICAL_SURFACE ( 'NONE', #1347, 7.500000000000000000, 0.7853981633974447263 ) ;
#3907 = CARTESIAN_POINT ( 'NONE',  ( -34.99999999999999289, -5.000000000000000000, -3.012171160963566127E-14 ) ) ;
#3908 = CYLINDRICAL_SURFACE ( 'NONE', #3989, 15.00000000000000000 ) ;
#3909 = VERTEX_POINT ( 'NONE', #7192 ) ;
#3910 = CARTESIAN_POINT ( 'NONE',  ( 5.999999999999998224, 20.00000000000000000, -5.999999999999999112 ) ) ;
#3911 = CARTESIAN_POINT ( 'NONE',  ( -6.094648662765727920, 40.00000000000000000, 52.13898825983068974 ) ) ;
#3912 = EDGE_LOOP ( 'NONE', ( #4536, #17484, #16535, #851 ) ) ;
#3913 = FACE_OUTER_BOUND ( 'NONE', #19433, .T. ) ;
#3914 = CARTESIAN_POINT ( 'NONE',  ( 2.775557561562891351E-14, -2.775557561562891351E-14, 2.999999999999999112 ) ) ;
#3915 = CARTESIAN_POINT ( 'NONE',  ( 19.46387463785189809, 8.808008015900604448, -57.95411844647834698 ) ) ;
#3916 = DIRECTION ( 'NONE',  ( 0.000000000000000000, -1.000000000000000000, 0.000000000000000000 ) ) ;
#3917 = EDGE_LOOP ( 'NONE', ( #5908, #632, #4245, #5770 ) ) ;
#3918 = CARTESIAN_POINT ( 'NONE',  ( -6.070730550690822902, -31.88709182564697286, -2.999999999999971578 ) ) ;
#3919 = DIRECTION ( 'NONE',  ( -1.296372316667914327E-16, -1.000000000000000000, 0.000000000000000000 ) ) ;
#3920 = VECTOR ( 'NONE', #22353, 1000.000000000000000 ) ;
#3921 = EDGE_CURVE ( 'NONE', #6468, #19936, #14844, .T. ) ;
#3922 = ORIENTED_EDGE ( 'NONE', *, *, #4411, .T. ) ;
#3923 = CARTESIAN_POINT ( 'NONE',  ( 12.84005703549854616, 1.693876179613353017, 55.76322220629359094 ) ) ;
#3924 = LINE ( 'NONE', #21329, #1310 ) ;
#3925 = CARTESIAN_POINT ( 'NONE',  ( 18.83615802559796037, -32.14641817400193702, 2.999999999999995559 ) ) ;
#3926 = AXIS2_PLACEMENT_3D ( 'NONE', #15020, #12966, #733 ) ;
#3927 = EDGE_CURVE ( 'NONE', #3415, #8689, #19240, .T. ) ;
#3928 = VERTEX_POINT ( 'NONE', #7081 ) ;
#3930 = VERTEX_POINT ( 'NONE', #19360 ) ;
#3929 = B_SPLINE_CURVE_WITH_KNOTS ( 'NONE', 3,
 ( #19236, #9022, #10503, #17508 ),
 .UNSPECIFIED., .F., .F.,
 ( 4, 4 ),
 ( 9.545285768588289738E-07, 0.001900595205834635509 ),
 .UNSPECIFIED. ) ;
#3931 = ORIENTED_EDGE ( 'NONE', *, *, #17148, .F. ) ;
#3932 = EDGE_CURVE ( 'NONE', #20230, #4376, #10098, .T. ) ;
#3933 = ORIENTED_EDGE ( 'NONE', *, *, #14294, .T. ) ;
#3934 = CARTESIAN_POINT ( 'NONE',  ( 19.99999999999998579, 20.00000000000000000, 60.62177826491070221 ) ) ;
#3935 = DIRECTION ( 'NONE',  ( 0.000000000000000000, 1.000000000000000000, 0.000000000000000000 ) ) ;
#3936 = CARTESIAN_POINT ( 'NONE',  ( -3.777351397511341336E-15, 39.99999999999997158, -48.73397172404481381 ) ) ;
#3937 = CARTESIAN_POINT ( 'NONE',  ( 7.287850628716163293, 40.00000000000000711, 52.67053206792662934 ) ) ;
#3938 = ORIENTED_EDGE ( 'NONE', *, *, #15815, .F. ) ;
#3939 = DIRECTION ( 'NONE',  ( 6.505213034913038160E-19, 3.903127820947822896E-18, 1.000000000000000000 ) ) ;
#3940 = DIRECTION ( 'NONE',  ( 1.000000000000000000, 0.000000000000000000, 0.000000000000000000 ) ) ;
#3941 = VERTEX_POINT ( 'NONE', #425 ) ;
#3942 = CARTESIAN_POINT ( 'NONE',  ( -8.485281374238560659, 28.19616000222403684, -3.000000000000000000 ) ) ;
#3943 = CARTESIAN_POINT ( 'NONE',  ( -22.41121774633938912, 19.23761757294739283, -58.66449182057564116 ) ) ;
#3944 = ADVANCED_FACE ( 'NONE', ( #3664 ), #10615, .F. ) ;
#3945 = DIRECTION ( 'NONE',  ( 0.000000000000000000, 0.7071067811865474617, 0.7071067811865474617 ) ) ;
#3946 = ORIENTED_EDGE ( 'NONE', *, *, #3921, .T. ) ;
#3947 = CARTESIAN_POINT ( 'NONE',  ( -18.22261011550271803, -31.92986134326270076, 2.800654218530509443 ) ) ;
#3948 = VECTOR ( 'NONE', #21942, 1000.000000000000000 ) ;
#3949 = VERTEX_POINT ( 'NONE', #1927 ) ;
#3950 = CARTESIAN_POINT ( 'NONE',  ( 34.24928931925771991, -6.742883674876576805, -2.999999999999971578 ) ) ;
#3951 = FACE_OUTER_BOUND ( 'NONE', #17332, .T. ) ;
#3952 = CARTESIAN_POINT ( 'NONE',  ( 14.67611967928950101, -31.67162468656004037, -2.999999999999995559 ) ) ;
#3953 = VERTEX_POINT ( 'NONE', #8910 ) ;
#3954 = CARTESIAN_POINT ( 'NONE',  ( 32.35999952201606789, -1.423424233832765173, 2.999999999999999112 ) ) ;
#3955 = VECTOR ( 'NONE', #12617, 1000.000000000000000 ) ;
#3956 = CIRCLE ( 'NONE', #5048, 34.90673715956759082 ) ;
#3957 = CARTESIAN_POINT ( 'NONE',  ( 18.02527238916047381, 28.84533800490727629, 60.11925852858798436 ) ) ;
#3958 = CARTESIAN_POINT ( 'NONE',  ( -1.423424233832348840, -32.35999952201618157, -6.999999999999992006 ) ) ;
#3959 = AXIS2_PLACEMENT_3D ( 'NONE', #16692, #16228, #11072 ) ;
#3960 = CARTESIAN_POINT ( 'NONE',  ( 13.23602284716676358, 35.01773851405933868, -58.53880247431292361 ) ) ;
#3961 = EDGE_LOOP ( 'NONE', ( #12443, #21933, #14021, #5013 ) ) ;
#3962 = EDGE_LOOP ( 'NONE', ( #5065, #20527 ) ) ;
#3963 = AXIS2_PLACEMENT_3D ( 'NONE', #9358, #2142, #12886 ) ;
#3964 = ORIENTED_EDGE ( 'NONE', *, *, #10073, .F. ) ;
#3965 = B_SPLINE_CURVE_WITH_KNOTS ( 'NONE', 3,
 ( #1586, #10053, #17165, #20732, #4918, #17273, #20502, #5036, #8463, #12021, #13834, #3429, #17054, #15432, #19015, #1478, #18780, #20394, #6747, #18898, #8575, #11893 ),
 .UNSPECIFIED., .F., .F.,
 ( 4, 2, 2, 2, 2, 2, 2, 2, 2, 2, 4 ),
 ( 0.007712149587921395336, 0.01231940472852629045, 0.01347121851367751727, 0.01462303229882874062, 0.01692665986913119425, 0.01807847365428242453, 0.01923028743943365482, 0.02153391500973611539, 0.02268572879488733873, 0.02383754258003856208, 0.02614117015034102265 ),
 .UNSPECIFIED. ) ;
#3966 = EDGE_CURVE ( 'NONE', #11046, #17302, #21180, .T. ) ;
#3967 = VERTEX_POINT ( 'NONE', #19463 ) ;
#3968 = CARTESIAN_POINT ( 'NONE',  ( 42.50000000000000711, -12.00000000000000000, -47.50000000000000000 ) ) ;
#3969 = CARTESIAN_POINT ( 'NONE',  ( -10.81645871527333114, 39.16817317915248253, -54.94897387134643196 ) ) ;
#3970 = VECTOR ( 'NONE', #19241, 1000.000000000000000 ) ;
#3971 = CARTESIAN_POINT ( 'NONE',  ( -1.387778780781445518E-14, 20.00000000000000355, -105.0000000000000142 ) ) ;
#3972 = CIRCLE ( 'NONE', #4330, 2.499999999999998668 ) ;
#3973 = EDGE_LOOP ( 'NONE', ( #6740, #403, #15276, #5398 ) ) ;
#3974 = DIRECTION ( 'NONE',  ( 6.505213034913038160E-19, 3.903127820947822896E-18, 1.000000000000000000 ) ) ;
#3975 = DIRECTION ( 'NONE',  ( 0.000000000000000000, 1.000000000000000000, 0.000000000000000000 ) ) ;
#3976 = AXIS2_PLACEMENT_3D ( 'NONE', #8325, #2836, #6606 ) ;
#3977 = ADVANCED_FACE ( 'NONE', ( #3768 ), #16007, .T. ) ;
#3978 = ORIENTED_EDGE ( 'NONE', *, *, #19823, .T. ) ;
#3979 = CARTESIAN_POINT ( 'NONE',  ( 24.41514043009201984, 26.50842683089762986, -2.999999999999947153 ) ) ;
#3980 = CARTESIAN_POINT ( 'NONE',  ( 42.50000000000000711, -12.00000000000000000, 47.50000000000000711 ) ) ;
#3981 = CARTESIAN_POINT ( 'NONE',  ( -33.46652738560673868, 11.93772187171645172, -3.000000000000015099 ) ) ;
#3982 = AXIS2_PLACEMENT_3D ( 'NONE', #19031, #18371, #2688 ) ;
#3983 = DIRECTION ( 'NONE',  ( 6.505213034913038160E-19, 3.903127820947822896E-18, 1.000000000000000000 ) ) ;
#3984 = AXIS2_PLACEMENT_3D ( 'NONE', #12211, #19213, #19095 ) ;
#3985 = CIRCLE ( 'NONE', #5431, 41.00000000000000000 ) ;
#3986 = CARTESIAN_POINT ( 'NONE',  ( -5.702716825709945425, 39.17357718829533297, 54.58701425223461712 ) ) ;
#3987 = EDGE_CURVE ( 'NONE', #4421, #6249, #15199, .T. ) ;
#3988 = CARTESIAN_POINT ( 'NONE',  ( 28.88846368933370456, 19.59430950039303809, -2.999999999999975131 ) ) ;
#3989 = AXIS2_PLACEMENT_3D ( 'NONE', #1949, #7334, #5502 ) ;
#3990 = ORIENTED_EDGE ( 'NONE', *, *, #12780, .T. ) ;
#3991 = VERTEX_POINT ( 'NONE', #13233 ) ;
#3992 = EDGE_CURVE ( 'NONE', #11258, #922, #6090, .T. ) ;
#3993 = ORIENTED_EDGE ( 'NONE', *, *, #17293, .T. ) ;
#3994 = DIRECTION ( 'NONE',  ( -1.000000000000000000, 1.371829164384562918E-16, 0.000000000000000000 ) ) ;
#3995 =( GEOMETRIC_REPRESENTATION_CONTEXT ( 3 ) GLOBAL_UNCERTAINTY_ASSIGNED_CONTEXT ( ( #5978 ) ) GLOBAL_UNIT_ASSIGNED_CONTEXT ( ( #6729, #21162, #15867 ) ) REPRESENTATION_CONTEXT ( 'NONE', 'WORKASPACE' ) );
#3996 = AXIS2_PLACEMENT_3D ( 'NONE', #4739, #4618, #18250 ) ;
#3997 = CARTESIAN_POINT ( 'NONE',  ( -28.95348479018550236, 14.76298474240492276, -6.999999999999950262 ) ) ;
#3998 = CARTESIAN_POINT ( 'NONE',  ( 5.511499161258694102, 0.6970817516955201132, -52.42185088606010623 ) ) ;
#3999 = DIRECTION ( 'NONE',  ( 0.000000000000000000, 0.000000000000000000, 1.000000000000000000 ) ) ;
#4000 = CARTESIAN_POINT ( 'NONE',  ( 17.32050807568880657, -1.500000000000015987, -9.999999999999934275 ) ) ;
#4001 = PLANE ( 'NONE',  #6171 ) ;
#4002 = CARTESIAN_POINT ( 'NONE',  ( -15.39832585462821868, 32.77960222724827588, -56.73873823673314831 ) ) ;
#4003 = PRODUCT_DEFINITION_FORMATION_WITH_SPECIFIED_SOURCE ( 'ANY', '', #20116, .NOT_KNOWN. ) ;
#4004 = CARTESIAN_POINT ( 'NONE',  ( 20.00000000000000000, 28.19616000222403329, 2.449293598294705724E-15 ) ) ;
#4005 = PRODUCT_DEFINITION_SHAPE ( 'NONE', 'NONE',  #18657 ) ;
#4006 = VERTEX_POINT ( 'NONE', #12899 ) ;
#4007 = DIRECTION ( 'NONE',  ( 1.000000000000000000, 0.000000000000000000, 0.000000000000000000 ) ) ;
#4008 = FACE_BOUND ( 'NONE', #9604, .T. ) ;
#4009 = CARTESIAN_POINT ( 'NONE',  ( -3.210598435713526211, 39.75302854575187439, -52.30739040051270905 ) ) ;
#4010 = ADVANCED_FACE ( 'NONE', ( #661 ), #13131, .F. ) ;
#4011 = DIRECTION ( 'NONE',  ( -0.000000000000000000, 1.000000000000000000, -0.000000000000000000 ) ) ;
#4012 = DIRECTION ( 'NONE',  ( -0.000000000000000000, -1.000000000000000000, -0.000000000000000000 ) ) ;
#4013 = ORIENTED_EDGE ( 'NONE', *, *, #18989, .T. ) ;
#4014 = CARTESIAN_POINT ( 'NONE',  ( -9.999999999999998224, 12.49999999999999822, 3.000000000000000000 ) ) ;
#4015 = ORIENTED_EDGE ( 'NONE', *, *, #12837, .F. ) ;
#4016 = EDGE_CURVE ( 'NONE', #14214, #8612, #16697, .T. ) ;
#4017 = AXIS2_PLACEMENT_3D ( 'NONE', #9577, #2712, #20128 ) ;
#4018 = CYLINDRICAL_SURFACE ( 'NONE', #14043, 2.999999999999999112 ) ;
#4019 = FACE_OUTER_BOUND ( 'NONE', #22566, .T. ) ;
#4020 = CARTESIAN_POINT ( 'NONE',  ( 14.30107462755360537, 5.991811841696046415, -58.93430465799249163 ) ) ;
#4021 = ADVANCED_FACE ( 'NONE', ( #18302 ), #4564, .F. ) ;
#4022 = EDGE_CURVE ( 'NONE', #2292, #11397, #17795, .T. ) ;
#4023 = VERTEX_POINT ( 'NONE', #14625 ) ;
#4024 = CARTESIAN_POINT ( 'NONE',  ( 35.00000000000001421, -5.000000000000000000, 1.540743955509788682E-30 ) ) ;
#4025 = CONTEXT_DEPENDENT_SHAPE_REPRESENTATION ( #18085, #713 ) ;
#4026 = EDGE_CURVE ( 'NONE', #22156, #7926, #19958, .T. ) ;
#4027 = ORIENTED_EDGE ( 'NONE', *, *, #17960, .T. ) ;
#4028 = CARTESIAN_POINT ( 'NONE',  ( -2.673152730111970410, 23.56975547524771741, 8.612623190900162484 ) ) ;
#4029 = FACE_OUTER_BOUND ( 'NONE', #21345, .T. ) ;
#4030 = VECTOR ( 'NONE', #11661, 1000.000000000000000 ) ;
#4031 = FACE_OUTER_BOUND ( 'NONE', #1522, .T. ) ;
#4032 = EDGE_CURVE ( 'NONE', #6302, #8864, #2842, .T. ) ;
#4033 = CARTESIAN_POINT ( 'NONE',  ( -34.99999999999999289, 4.000000000000028422, -3.012171160963566127E-14 ) ) ;
#4034 = CARTESIAN_POINT ( 'NONE',  ( -8.219889501007404675, 1.750964516535594040, -56.08920281152427378 ) ) ;
#4035 = ORIENTED_EDGE ( 'NONE', *, *, #19026, .T. ) ;
#4036 = CARTESIAN_POINT ( 'NONE',  ( 3.330669073875469621E-13, -1.110223024625156540E-13, -2.999999999999971578 ) ) ;
#4037 = DIRECTION ( 'NONE',  ( 1.000000000000000000, 1.208970125616063028E-17, 0.000000000000000000 ) ) ;
#4038 = CARTESIAN_POINT ( 'NONE',  ( -9.505536299094565322, 39.99999999999999289, 53.50900092114397921 ) ) ;
#4039 = CARTESIAN_POINT ( 'NONE',  ( 25.00000000000000000, 20.00000000000000000, 6.487780019669002523E-15 ) ) ;
#4040 = VERTEX_POINT ( 'NONE', #11316 ) ;
#4041 = LINE ( 'NONE', #9625, #22591 ) ;
#4042 = CARTESIAN_POINT ( 'NONE',  ( -8.219889500999224552, 1.750964516532281356, 56.08920281153879017 ) ) ;
#4043 = CARTESIAN_POINT ( 'NONE',  ( -0.2640866027062644950, 39.99958921875370521, -48.93844571589828263 ) ) ;
#4044 = VERTEX_POINT ( 'NONE', #4106 ) ;
#4045 = AXIS2_PLACEMENT_3D ( 'NONE', #4585, #14758, #20282 ) ;
#4046 = DIRECTION ( 'NONE',  ( 0.000000000000000000, 1.000000000000000000, 0.000000000000000000 ) ) ;
#4047 = ORIENTED_EDGE ( 'NONE', *, *, #9212, .T. ) ;
#4048 = ORIENTED_EDGE ( 'NONE', *, *, #12656, .F. ) ;
#4049 = EDGE_LOOP ( 'NONE', ( #12134, #11751 ) ) ;
#4050 = ADVANCED_FACE ( 'NONE', ( #11541 ), #20031, .F. ) ;
#4051 = ORIENTED_EDGE ( 'NONE', *, *, #20533, .F. ) ;
#4052 = DIRECTION ( 'NONE',  ( 6.505213034913038160E-19, 3.903127820947822896E-18, 1.000000000000000000 ) ) ;
#4053 = CARTESIAN_POINT ( 'NONE',  ( -8.485281374238564212, 1.499999999999997558, -3.000000000000000000 ) ) ;
#4054 = AXIS2_PLACEMENT_3D ( 'NONE', #11963, #3274, #19190 ) ;
#4055 = CARTESIAN_POINT ( 'NONE',  ( 1.486416059063909278, 39.99051308249325842, -49.86506293652772115 ) ) ;
#4056 = EDGE_CURVE ( 'NONE', #18787, #13935, #2382, .T. ) ;
#4057 = DIRECTION ( 'NONE',  ( 0.000000000000000000, 0.000000000000000000, 1.000000000000000000 ) ) ;
#4058 = ORIENTED_EDGE ( 'NONE', *, *, #10987, .F. ) ;
#4059 = CARTESIAN_POINT ( 'NONE',  ( 5.833333333333329485, 40.00000000000000000, -40.61164310337066041 ) ) ;
#4060 = CARTESIAN_POINT ( 'NONE',  ( -34.74700806321090596, 12.00937115242645170, 2.800654218530481465 ) ) ;
#4061 = EDGE_LOOP ( 'NONE', ( #18011, #5121, #2523, #959 ) ) ;
#4062 = DIRECTION ( 'NONE',  ( 6.505213034913038160E-19, 3.903127820947822896E-18, 1.000000000000000000 ) ) ;
#4063 = CARTESIAN_POINT ( 'NONE',  ( -89.99999999999701572, 0.000000000000000000, 2.499999999999978684 ) ) ;
#4064 = VERTEX_POINT ( 'NONE', #18874 ) ;
#4065 = CARTESIAN_POINT ( 'NONE',  ( 2.589862425843441063, 0.1394011931331439469, 50.61994180263811671 ) ) ;
#4066 = EDGE_CURVE ( 'NONE', #18872, #19255, #4263, .T. ) ;
#4067 = ORIENTED_EDGE ( 'NONE', *, *, #4272, .F. ) ;
#4068 = CARTESIAN_POINT ( 'NONE',  ( 8.970852013922840484, 37.88903915979515347, 54.67447700193728366 ) ) ;
#4069 = DIRECTION ( 'NONE',  ( 1.000000000000000000, 0.000000000000000000, 0.000000000000000000 ) ) ;
#4070 = CARTESIAN_POINT ( 'NONE',  ( 14.85562396683509689, -32.28023859650878080, -2.999999999999985789 ) ) ;
#4071 = ORIENTED_EDGE ( 'NONE', *, *, #688, .F. ) ;
#4072 = CARTESIAN_POINT ( 'NONE',  ( 22.20997089757253207, 23.22761694305071245, 58.62102808997010328 ) ) ;
#4073 = DIRECTION ( 'NONE',  ( -1.000000000000000000, -1.208970125616063644E-17, 0.000000000000000000 ) ) ;
#4074 = VECTOR ( 'NONE', #2557, 1000.000000000000000 ) ;
#4075 = CARTESIAN_POINT ( 'NONE',  ( 13.87722263113801802, 34.42803545437053003, -58.77926695580346461 ) ) ;
#4076 = ORIENTED_EDGE ( 'NONE', *, *, #7958, .F. ) ;
#4077 = EDGE_CURVE ( 'NONE', #12705, #3042, #13810, .T. ) ;
#4078 = ORIENTED_EDGE ( 'NONE', *, *, #22403, .T. ) ;
#4079 = ORIENTED_EDGE ( 'NONE', *, *, #14617, .F. ) ;
#4080 = VERTEX_POINT ( 'NONE', #10264 ) ;
#4081 = CARTESIAN_POINT ( 'NONE',  ( 0.000000000000000000, 15.00000000000000000, 0.000000000000000000 ) ) ;
#4082 = CARTESIAN_POINT ( 'NONE',  ( -10.08226496024166430, 39.27879523455747091, -54.68359763800749818 ) ) ;
#4083 = CARTESIAN_POINT ( 'NONE',  ( -34.99999999999980815, 40.00000000000000711, 54.99999999999922551 ) ) ;
#4084 = ORIENTED_EDGE ( 'NONE', *, *, #12745, .F. ) ;
#4085 = DIRECTION ( 'NONE',  ( 0.000000000000000000, 1.000000000000000000, 0.000000000000000000 ) ) ;
#4086 = CARTESIAN_POINT ( 'NONE',  ( -3.235223465815322719, -4.647308930658608617, 47.76313845446109951 ) ) ;
#4087 = ORIENTED_EDGE ( 'NONE', *, *, #17634, .F. ) ;
#4088 = DIRECTION ( 'NONE',  ( -0.000000000000000000, -1.000000000000000000, -0.000000000000000000 ) ) ;
#4089 = DIRECTION ( 'NONE',  ( -0.000000000000000000, -1.000000000000000000, -0.000000000000000000 ) ) ;
#4090 = DIRECTION ( 'NONE',  ( -0.000000000000000000, 1.000000000000000000, -0.000000000000000000 ) ) ;
#4091 = DIRECTION ( 'NONE',  ( -0.000000000000000000, -0.000000000000000000, -1.000000000000000000 ) ) ;
#4092 = CARTESIAN_POINT ( 'NONE',  ( 35.00000000000058265, 39.97500000000000142, -55.00000000000076028 ) ) ;
#4093 = EDGE_CURVE ( 'NONE', #12118, #17505, #9376, .T. ) ;
#4094 = CIRCLE ( 'NONE', #9200, 2.099999999999997868 ) ;
#4095 = DIRECTION ( 'NONE',  ( -0.000000000000000000, -0.000000000000000000, -1.000000000000000000 ) ) ;
#4096 = DIRECTION ( 'NONE',  ( -1.000000000000000000, -1.788446540656407938E-15, 0.000000000000000000 ) ) ;
#4097 = VERTEX_POINT ( 'NONE', #6384 ) ;
#4098 = ADVANCED_FACE ( 'NONE', ( #16922 ), #20728, .T. ) ;
#4099 = ORIENTED_EDGE ( 'NONE', *, *, #21744, .F. ) ;
#4100 = ORIENTED_EDGE ( 'NONE', *, *, #6274, .F. ) ;
#4101 = CARTESIAN_POINT ( 'NONE',  ( -35.00000000000000000, 25.00000000000000000, 2.365113165210053967E-14 ) ) ;
#4102 = FACE_OUTER_BOUND ( 'NONE', #4209, .T. ) ;
#4103 = CARTESIAN_POINT ( 'NONE',  ( 4.664549341139476724, 0.4975632029830715508, -53.81030450292873013 ) ) ;
#4104 = AXIS2_PLACEMENT_3D ( 'NONE', #11985, #5007, #5229 ) ;
#4105 = EDGE_CURVE ( 'NONE', #16638, #11727, #16321, .T. ) ;
#4106 = CARTESIAN_POINT ( 'NONE',  ( -8.485281374238564212, 12.49999999999999822, 3.000000000000000000 ) ) ;
#4107 = FACE_OUTER_BOUND ( 'NONE', #6243, .T. ) ;
#4108 = CARTESIAN_POINT ( 'NONE',  ( -2.039347869096966038E-14, 40.00000000000000000, -48.73397172404482092 ) ) ;
#4109 = CARTESIAN_POINT ( 'NONE',  ( -25.58633464742622721, -23.74488952252778873, 3.000000000000002665 ) ) ;
#4110 = CARTESIAN_POINT ( 'NONE',  ( -35.33352588067073441, -7.094908322883425100, -7.000000000000006217 ) ) ;
#4111 = ORIENTED_EDGE ( 'NONE', *, *, #13673, .T. ) ;
#4112 = FACE_BOUND ( 'NONE', #15145, .T. ) ;
#4113 = CARTESIAN_POINT ( 'NONE',  ( -42.50000000000000711, -12.00000000000000000, -47.50000000000000000 ) ) ;
#4114 = DIRECTION ( 'NONE',  ( 0.000000000000000000, 0.000000000000000000, -1.000000000000000000 ) ) ;
#4115 = EDGE_CURVE ( 'NONE', #19351, #5750, #19686, .T. ) ;
#4116 = FACE_OUTER_BOUND ( 'NONE', #19797, .T. ) ;
#4117 = VERTEX_POINT ( 'NONE', #7716 ) ;
#4118 = CARTESIAN_POINT ( 'NONE',  ( 27.19760187735889545, 24.73600648735091312, 2.800654218530485018 ) ) ;
#4119 = CYLINDRICAL_SURFACE ( 'NONE', #9690, 2.499999999999996891 ) ;
#4120 = FACE_OUTER_BOUND ( 'NONE', #3156, .T. ) ;
#4121 = FACE_OUTER_BOUND ( 'NONE', #5496, .T. ) ;
#4122 = CIRCLE ( 'NONE', #5234, 28.00000000000000355 ) ;
#4123 = VERTEX_POINT ( 'NONE', #19336 ) ;
#4124 = CARTESIAN_POINT ( 'NONE',  ( -90.00000000000000000, 26.00000000000000355, 2.099999999999989875 ) ) ;
#4125 = CYLINDRICAL_SURFACE ( 'NONE', #9423, 2.500000000000002220 ) ;
#4126 = ORIENTED_EDGE ( 'NONE', *, *, #7210, .F. ) ;
#4127 = CARTESIAN_POINT ( 'NONE',  ( 9.177445128772406591, 39.41890422686074658, -54.36989725583298849 ) ) ;
#4128 = DIRECTION ( 'NONE',  ( 1.000000000000000000, 0.000000000000000000, 0.000000000000000000 ) ) ;
#4129 = EDGE_CURVE ( 'NONE', #10068, #18626, #8283, .T. ) ;
#4130 = DIRECTION ( 'NONE',  ( 0.000000000000000000, 0.000000000000000000, -1.000000000000000000 ) ) ;
#4131 = VERTEX_POINT ( 'NONE', #19979 ) ;
#4132 = DIRECTION ( 'NONE',  ( 0.000000000000000000, -0.000000000000000000, 1.000000000000000000 ) ) ;
#4133 = DIRECTION ( 'NONE',  ( -6.505213034913038160E-19, -3.903127820947822896E-18, -1.000000000000000000 ) ) ;
#4134 = ORIENTED_EDGE ( 'NONE', *, *, #12249, .F. ) ;
#4135 = DIRECTION ( 'NONE',  ( -6.505213034913038160E-19, -3.903127820947822896E-18, -1.000000000000000000 ) ) ;
#4136 = CARTESIAN_POINT ( 'NONE',  ( 2.775557561562891351E-14, -2.775557561562891351E-14, 2.999999999999999112 ) ) ;
#4137 = CARTESIAN_POINT ( 'NONE',  ( -34.99999999999999289, 0.000000000000000000, -3.012171160963566127E-14 ) ) ;
#4138 = EDGE_LOOP ( 'NONE', ( #20614, #21838 ) ) ;
#4139 = CARTESIAN_POINT ( 'NONE',  ( -20.00948735876882623, -24.79619811426206510, -6.999999999999950262 ) ) ;
#4140 = DIRECTION ( 'NONE',  ( 0.000000000000000000, 0.000000000000000000, 1.000000000000000000 ) ) ;
#4141 = ADVANCED_FACE ( 'NONE', ( #20938 ), #10486, .F. ) ;
#4142 = EDGE_CURVE ( 'NONE', #4270, #11307, #15950, .T. ) ;
#4143 = CARTESIAN_POINT ( 'NONE',  ( -4.273193112870391275, 39.88698587828563547, -51.75894944362807593 ) ) ;
#4144 = CIRCLE ( 'NONE', #16935, 31.50000000000000711 ) ;
#4145 = EDGE_CURVE ( 'NONE', #18626, #6724, #12968, .T. ) ;
#4146 = VERTEX_POINT ( 'NONE', #14257 ) ;
#4147 = DIRECTION ( 'NONE',  ( 1.296372316667914327E-16, 1.000000000000000000, -0.000000000000000000 ) ) ;
#4148 = DIRECTION ( 'NONE',  ( 0.000000000000000000, 0.000000000000000000, 1.000000000000000000 ) ) ;
#4149 = DIRECTION ( 'NONE',  ( -1.000000000000000000, 0.000000000000000000, 0.000000000000000000 ) ) ;
#4150 = EDGE_CURVE ( 'NONE', #5303, #817, #2568, .T. ) ;
#4151 = VERTEX_POINT ( 'NONE', #19448 ) ;
#4152 = AXIS2_PLACEMENT_3D ( 'NONE', #12645, #16201, #511 ) ;
#4153 = ORIENTED_EDGE ( 'NONE', *, *, #15425, .T. ) ;
#4154 = ORIENTED_EDGE ( 'NONE', *, *, #10758, .F. ) ;
#4155 =( NAMED_UNIT ( * ) PLANE_ANGLE_UNIT ( ) SI_UNIT ( $, .RADIAN. ) );
#4156 = ORIENTED_EDGE ( 'NONE', *, *, #19194, .F. ) ;
#4157 = FACE_BOUND ( 'NONE', #9390, .T. ) ;
#4158 = DIRECTION ( 'NONE',  ( -0.000000000000000000, -0.000000000000000000, -1.000000000000000000 ) ) ;
#4159 = CARTESIAN_POINT ( 'NONE',  ( 1.387778780781445676E-14, 40.00000000000000000, 48.73397172404482802 ) ) ;
#4160 = DIRECTION ( 'NONE',  ( -0.000000000000000000, -0.000000000000000000, 1.000000000000000000 ) ) ;
#4161 = CARTESIAN_POINT ( 'NONE',  ( 10.49999999999994316, 42.51666049839543149, -105.0010000000000048 ) ) ;
#4162 = ORIENTED_EDGE ( 'NONE', *, *, #2005, .F. ) ;
#4163 = CARTESIAN_POINT ( 'NONE',  ( -34.99999999999999289, 0.000000000000000000, -11.00000000000006750 ) ) ;
#4164 = CARTESIAN_POINT ( 'NONE',  ( -25.00000000000000000, 20.00000000000000000, -16.49999999999998934 ) ) ;
#4165 = ORIENTED_EDGE ( 'NONE', *, *, #2705, .F. ) ;
#4166 = CARTESIAN_POINT ( 'NONE',  ( 2.220446049250313081E-13, -8.326672684688674053E-14, 2.800654218530498785 ) ) ;
#4167 = CARTESIAN_POINT ( 'NONE',  ( 10.50000000000024514, -2.516660498395250301, 105.0000000000000142 ) ) ;
#4168 = DIRECTION ( 'NONE',  ( 1.000000000000000000, 0.000000000000000000, 0.000000000000000000 ) ) ;
#4169 = ORIENTED_EDGE ( 'NONE', *, *, #21574, .F. ) ;
#4170 = CARTESIAN_POINT ( 'NONE',  ( 19.99999999999998579, 20.00000000000000355, -98.00000000000000000 ) ) ;
#4171 = ORIENTED_EDGE ( 'NONE', *, *, #2028, .F. ) ;
#4172 = CARTESIAN_POINT ( 'NONE',  ( 6.869621667053231739, 39.72564009089534665, 53.24680777370071638 ) ) ;
#4173 = FACE_OUTER_BOUND ( 'NONE', #135, .T. ) ;
#4174 = CYLINDRICAL_SURFACE ( 'NONE', #20983, 1.000000000000000888 ) ;
#4175 = ORIENTED_EDGE ( 'NONE', *, *, #13148, .F. ) ;
#4176 = CARTESIAN_POINT ( 'NONE',  ( -35.00000000000000000, 10.00000000000000000, -40.99999999999997868 ) ) ;
#4177 = VECTOR ( 'NONE', #2476, 999.9999999999998863 ) ;
#4178 = DIRECTION ( 'NONE',  ( 0.000000000000000000, 0.000000000000000000, 1.000000000000000000 ) ) ;
#4179 = CARTESIAN_POINT ( 'NONE',  ( -15.50000000000011013, 42.51666049839536043, 105.0000000000000142 ) ) ;
#4180 = CIRCLE ( 'NONE', #10015, 17.00000000000000000 ) ;
#4181 = CIRCLE ( 'NONE', #6007, 36.76383501243555685 ) ;
#4182 = EDGE_CURVE ( 'NONE', #5980, #4044, #8889, .T. ) ;
#4183 = EDGE_CURVE ( 'NONE', #3398, #20205, #13753, .T. ) ;
#4184 = FACE_BOUND ( 'NONE', #8347, .T. ) ;
#4185 = EDGE_LOOP ( 'NONE', ( #15540, #1052, #9663, #13067 ) ) ;
#4186 = ORIENTED_EDGE ( 'NONE', *, *, #10227, .T. ) ;
#4187 = EDGE_CURVE ( 'NONE', #7505, #2375, #5722, .T. ) ;
#4188 = ORIENTED_EDGE ( 'NONE', *, *, #14281, .T. ) ;
#4189 = VERTEX_POINT ( 'NONE', #4288 ) ;
#4190 = CARTESIAN_POINT ( 'NONE',  ( -1.387778780781445676E-14, 20.00000000000000000, -100.0000000000000000 ) ) ;
#4191 = CARTESIAN_POINT ( 'NONE',  ( -10.49999999999980460, -2.516660498395516310, -105.0010000000000048 ) ) ;
#4192 = CONICAL_SURFACE ( 'NONE', #6735, 22.12933039895921539, 1.308996938995746095 ) ;
#4193 = DIRECTION ( 'NONE',  ( 0.000000000000000000, 0.000000000000000000, 1.000000000000000000 ) ) ;
#4194 = ORIENTED_EDGE ( 'NONE', *, *, #5415, .F. ) ;
#4195 = CARTESIAN_POINT ( 'NONE',  ( -10.43027093729396526, 39.22757009021463404, -54.80615623442352558 ) ) ;
#4196 = DIRECTION ( 'NONE',  ( 0.9898477157360405787, 0.000000000000000000, 0.1421319796954322312 ) ) ;
#4197 = CIRCLE ( 'NONE', #22478, 15.99999999999998579 ) ;
#4198 = ORIENTED_EDGE ( 'NONE', *, *, #16916, .T. ) ;
#4199 = CARTESIAN_POINT ( 'NONE',  ( 11.99035502499705430, 39.33333333333332860, -55.05149724789898613 ) ) ;
#4200 = CARTESIAN_POINT ( 'NONE',  ( 6.070730550691017413, 31.88709182564680589, -2.999999999999995559 ) ) ;
#4201 = CARTESIAN_POINT ( 'NONE',  ( 35.00000000000001421, -5.000000000000000000, 1.540743955509788682E-30 ) ) ;
#4202 =( NAMED_UNIT ( * ) PLANE_ANGLE_UNIT ( ) SI_UNIT ( $, .RADIAN. ) );
#4203 = AXIS2_PLACEMENT_3D ( 'NONE', #4400, #9886, #4511 ) ;
#4204 = CARTESIAN_POINT ( 'NONE',  ( 28.73837443790554502, -21.94460005644937439, -2.932164912090501563 ) ) ;
#4205 = AXIS2_PLACEMENT_3D ( 'NONE', #9504, #14745, #2634 ) ;
#4206 = CARTESIAN_POINT ( 'NONE',  ( -3.244689583143795186, 39.74755540027226886, 52.34195286440937167 ) ) ;
#4207 = LINE ( 'NONE', #9480, #22214 ) ;
#4208 = ORIENTED_EDGE ( 'NONE', *, *, #10152, .F. ) ;
#4209 = EDGE_LOOP ( 'NONE', ( #11237, #6980, #15911, #7527 ) ) ;
#4210 = VERTEX_POINT ( 'NONE', #68 ) ;
#4211 = CARTESIAN_POINT ( 'NONE',  ( 35.00000000000002132, -5.000000000000000000, -59.99999999999703704 ) ) ;
#4212 = CARTESIAN_POINT ( 'NONE',  ( 35.00000000000000000, 40.00000000000000000, 4.258610482196280173E-15 ) ) ;
#4213 = EDGE_CURVE ( 'NONE', #16878, #10013, #2454, .T. ) ;
#4214 = VECTOR ( 'NONE', #19, 1000.000000000000000 ) ;
#4215 = CARTESIAN_POINT ( 'NONE',  ( 0.1564864144766087983, 40.00000000000000000, 48.92140276528778031 ) ) ;
#4216 = DIRECTION ( 'NONE',  ( 6.505213034913038160E-19, 3.903127820947822896E-18, 1.000000000000000000 ) ) ;
#4217 = CARTESIAN_POINT ( 'NONE',  ( -5.617742387210350685, 39.81211049013471381, -52.56498094152444622 ) ) ;
#4218 = DIRECTION ( 'NONE',  ( 0.000000000000000000, 0.000000000000000000, 1.000000000000000000 ) ) ;
#4219 = CARTESIAN_POINT ( 'NONE',  ( -22.97438720605730822, 22.98755168577401520, -7.000000000000006217 ) ) ;
#4220 = DIRECTION ( 'NONE',  ( -1.000000000000000000, 0.000000000000000000, 0.000000000000000000 ) ) ;
#4221 = EDGE_CURVE ( 'NONE', #19293, #16318, #9444, .T. ) ;
#4222 = ORIENTED_EDGE ( 'NONE', *, *, #10562, .T. ) ;
#4223 = B_SPLINE_CURVE_WITH_KNOTS ( 'NONE', 3,
 ( #9534, #8153, #20307, #7810, #2895, #18345, #15118, #9425, #4386, #11361, #7932, #2665 ),
 .UNSPECIFIED., .F., .F.,
 ( 4, 1, 1, 1, 1, 2, 2, 4 ),
 ( 0.000000000000000000, 0.2499999999999911182, 0.3749999999999869549, 0.4374999999999852340, 0.4687499999999832911, 0.4843749999999822919, 0.4999999999999812927, 1.000000000000000000 ),
 .UNSPECIFIED. ) ;
#4224 = CARTESIAN_POINT ( 'NONE',  ( 5.551115123125782702E-14, -1.387778780781445676E-13, -5.749999999999949374 ) ) ;
#4225 = CARTESIAN_POINT ( 'NONE',  ( -34.99999999999999289, -5.000000000000000000, -54.99999999999705125 ) ) ;
#4226 = CARTESIAN_POINT ( 'NONE',  ( 35.33352588067128863, 7.094908322883036966, -2.999999999999971578 ) ) ;
#4227 = VECTOR ( 'NONE', #12091, 1000.000000000000000 ) ;
#4228 = DIRECTION ( 'NONE',  ( -0.000000000000000000, -1.000000000000000000, -0.000000000000000000 ) ) ;
#4229 = ORIENTED_EDGE ( 'NONE', *, *, #4315, .T. ) ;
#4230 = LINE ( 'NONE', #2739, #17492 ) ;
#4231 = AXIS2_PLACEMENT_3D ( 'NONE', #7568, #457, #918 ) ;
#4232 = ORIENTED_EDGE ( 'NONE', *, *, #21498, .T. ) ;
#4233 = DIRECTION ( 'NONE',  ( 0.000000000000000000, -1.000000000000000000, 0.000000000000000000 ) ) ;
#4234 = LINE ( 'NONE', #7670, #19621 ) ;
#4235 = AXIS2_PLACEMENT_3D ( 'NONE', #7172, #21047, #9126 ) ;
#4236 = ORIENTED_EDGE ( 'NONE', *, *, #18376, .F. ) ;
#4237 = DIRECTION ( 'NONE',  ( 0.000000000000000000, 0.000000000000000000, -1.000000000000000000 ) ) ;
#4238 = CARTESIAN_POINT ( 'NONE',  ( 2.478389530992044065, 40.00000000000000000, -50.25195279936158954 ) ) ;
#4239 = CIRCLE ( 'NONE', #13000, 2.524999999999999467 ) ;
#4240 = ADVANCED_FACE ( 'NONE', ( #7170 ), #7604, .F. ) ;
#4241 = ORIENTED_EDGE ( 'NONE', *, *, #4066, .T. ) ;
#4242 = CARTESIAN_POINT ( 'NONE',  ( 2.105505840716530574, 39.97335763330380587, -50.30092836639100540 ) ) ;
#4243 = VECTOR ( 'NONE', #17120, 1000.000000000000000 ) ;
#4244 = FACE_OUTER_BOUND ( 'NONE', #3050, .T. ) ;
#4245 = ORIENTED_EDGE ( 'NONE', *, *, #22073, .T. ) ;
#4246 = CARTESIAN_POINT ( 'NONE',  ( 48.93401015228424455, 10.00000000000000000, -46.57614213197967956 ) ) ;
#4247 = FACE_OUTER_BOUND ( 'NONE', #18799, .T. ) ;
#4248 = ORIENTED_EDGE ( 'NONE', *, *, #22394, .T. ) ;
#4249 = AXIS2_PLACEMENT_3D ( 'NONE', #17632, #214, #19373 ) ;
#4250 = DIRECTION ( 'NONE',  ( -0.000000000000000000, -1.000000000000000000, -0.000000000000000000 ) ) ;
#4251 = LINE ( 'NONE', #5961, #22162 ) ;
#4252 = EDGE_CURVE ( 'NONE', #22506, #2582, #20413, .T. ) ;
#4253 = AXIS2_PLACEMENT_3D ( 'NONE', #11439, #2743, #2635 ) ;
#4254 = CARTESIAN_POINT ( 'NONE',  ( 35.00000000000001421, 0.000000000000000000, 1.540743955509788682E-30 ) ) ;
#4255 = ORIENTED_EDGE ( 'NONE', *, *, #18899, .T. ) ;
#4256 = DIRECTION ( 'NONE',  ( -0.000000000000000000, 1.000000000000000000, -0.000000000000000000 ) ) ;
#4257 = DIRECTION ( 'NONE',  ( 0.000000000000000000, 0.000000000000000000, -1.000000000000000000 ) ) ;
#4258 = CARTESIAN_POINT ( 'NONE',  ( -0.1139232394121202224, 39.99992693198588967, -48.82246310442314297 ) ) ;
#4259 = EDGE_LOOP ( 'NONE', ( #21771, #20997, #17156, #9624 ) ) ;
#4260 = DIRECTION ( 'NONE',  ( -1.000000000000000000, 0.000000000000000000, 0.000000000000000000 ) ) ;
#4261 = CARTESIAN_POINT ( 'NONE',  ( -1.387778780781445676E-14, 20.00000000000000000, -101.0000000000000284 ) ) ;
#4262 = AXIS2_PLACEMENT_3D ( 'NONE', #17067, #22359, #20622 ) ;
#4263 = CIRCLE ( 'NONE', #22573, 49.99999999999998579 ) ;
#4264 = CONICAL_SURFACE ( 'NONE', #6831, 2.099999999999997868, 1.029744258676652091 ) ;
#4265 = AXIS2_PLACEMENT_3D ( 'NONE', #16425, #3587, #14665 ) ;
#4266 = EDGE_CURVE ( 'NONE', #10013, #6602, #12283, .T. ) ;
#4267 = VERTEX_POINT ( 'NONE', #7059 ) ;
#4268 = CIRCLE ( 'NONE', #17059, 31.50000000000001421 ) ;
#4269 = ORIENTED_EDGE ( 'NONE', *, *, #16752, .T. ) ;
#4270 = VERTEX_POINT ( 'NONE', #21045 ) ;
#4271 = CARTESIAN_POINT ( 'NONE',  ( 0.000000000000000000, 0.000000000000000000, 0.000000000000000000 ) ) ;
#4272 = EDGE_CURVE ( 'NONE', #17695, #862, #16420, .T. ) ;
#4273 = EDGE_CURVE ( 'NONE', #10917, #1054, #3858, .T. ) ;
#4274 = ORIENTED_EDGE ( 'NONE', *, *, #1725, .T. ) ;
#4275 = FACE_OUTER_BOUND ( 'NONE', #4304, .T. ) ;
#4276 = DIRECTION ( 'NONE',  ( -0.000000000000000000, -1.000000000000000000, 0.000000000000000000 ) ) ;
#4277 = FACE_OUTER_BOUND ( 'NONE', #19436, .T. ) ;
#4278 = CARTESIAN_POINT ( 'NONE',  ( 1.833353995796188407, 5.110175324539462771, -38.89995731584652106 ) ) ;
#4279 = ORIENTED_EDGE ( 'NONE', *, *, #5478, .T. ) ;
#4280 = CARTESIAN_POINT ( 'NONE',  ( -41.39271818392636959, 10.00000000000000000, -5.943569790512535533 ) ) ;
#4281 = DIRECTION ( 'NONE',  ( -1.000000000000000000, -1.208970125616060717E-17, 0.000000000000000000 ) ) ;
#4282 = VERTEX_POINT ( 'NONE', #16405 ) ;
#4283 = CARTESIAN_POINT ( 'NONE',  ( -11.84374239103370741, 10.78799321809639800, -44.31542800769554447 ) ) ;
#4284 = AXIS2_PLACEMENT_3D ( 'NONE', #11457, #2538, #6199 ) ;
#4285 = CARTESIAN_POINT ( 'NONE',  ( 0.000000000000000000, -45.00000000000000000, 5.000000000000000000 ) ) ;
#4286 = CARTESIAN_POINT ( 'NONE',  ( 19.99999999999998579, 20.00000000000000711, -60.62177826491069510 ) ) ;
#4287 = ORIENTED_EDGE ( 'NONE', *, *, #20018, .T. ) ;
#4288 = CARTESIAN_POINT ( 'NONE',  ( -27.19760187735867518, -24.73600648735113694, -2.800654218530429507 ) ) ;
#4289 = CARTESIAN_POINT ( 'NONE',  ( -35.00000000000000000, 15.00000000000000000, 2.365113165210053967E-14 ) ) ;
#4290 = ORIENTED_EDGE ( 'NONE', *, *, #3552, .F. ) ;
#4291 = CARTESIAN_POINT ( 'NONE',  ( 8.957563853402323417, 39.56956388360624288, 54.21303480198576352 ) ) ;
#4292 = EDGE_CURVE ( 'NONE', #8817, #18681, #6505, .T. ) ;
#4293 = CIRCLE ( 'NONE', #4608, 6.499999999999999112 ) ;
#4294 = ORIENTED_EDGE ( 'NONE', *, *, #6266, .F. ) ;
#4295 = CYLINDRICAL_SURFACE ( 'NONE', #11531, 2.500000000000002220 ) ;
#4296 = CARTESIAN_POINT ( 'NONE',  ( 2.775557561562891351E-14, -2.775557561562891351E-14, 2.999999999999995559 ) ) ;
#4297 = EDGE_CURVE ( 'NONE', #17042, #6865, #20775, .T. ) ;
#4298 = DIRECTION ( 'NONE',  ( 1.049727191138617340E-16, 0.5150380749100560429, -0.8571673007021112234 ) ) ;
#4299 = EDGE_CURVE ( 'NONE', #14562, #15515, #14533, .T. ) ;
#4300 = VECTOR ( 'NONE', #18816, 1000.000000000000000 ) ;
#4301 = AXIS2_PLACEMENT_3D ( 'NONE', #17686, #19530, #2111 ) ;
#4302 = ORIENTED_EDGE ( 'NONE', *, *, #15059, .T. ) ;
#4303 = VERTEX_POINT ( 'NONE', #19750 ) ;
#4304 = EDGE_LOOP ( 'NONE', ( #13986, #10646, #8167, #15663 ) ) ;
#4305 = ADVANCED_FACE ( 'NONE', ( #21681 ), #2207, .F. ) ;
#4306 = EDGE_LOOP ( 'NONE', ( #6372, #8866, #818, #13623 ) ) ;
#4307 = DIRECTION ( 'NONE',  ( 6.505213034913038160E-19, 3.903127820947822896E-18, 1.000000000000000000 ) ) ;
#4308 = CARTESIAN_POINT ( 'NONE',  ( 4.163799117100996122E-16, 15.00000000000000000, -3.399999999999995914 ) ) ;
#4309 = DIRECTION ( 'NONE',  ( 0.000000000000000000, 0.000000000000000000, -1.000000000000000000 ) ) ;
#4310 =( BOUNDED_SURFACE ( )  B_SPLINE_SURFACE ( 3, 2, ( 
 ( #1485, #8363, #10061 ),
 ( #4925, #8469, #15438 ),
 ( #4816, #15332, #17171 ),
 ( #6639, #22350, #13599 ),
 ( #18905, #3212, #22460 ),
 ( #10178, #6756, #13492 ),
 ( #18786, #20509, #3091 ),
 ( #1367, #2832, #8212 ),
 ( #21978, #13568, #18645 ),
 ( #14837, #16807, #4442 ),
 ( #15171, #4783, #994 ),
 ( #15296, #7993, #22320 ),
 ( #16689, #22081, #20138 ),
 ( #2950, #9819, #6604 ),
 ( #878, #18748, #17020 ),
 ( #6268, #16912, #14953 ),
 ( #11754, #11416, #1330 ),
 ( #1112, #8321, #9699 ),
 ( #3054, #16572, #20580 ),
 ( #10028, #7870, #9924 ),
 ( #20476, #11308, #18297 ),
 ( #13124, #9585, #2609 ),
 ( #4555, #21860, #6160 ),
 ( #18400, #22197, #6375 ),
 ( #13227, #20248, #11534 ),
 ( #2723, #18521, #13338 ),
 ( #8103, #15061, #1212 ),
 ( #20365, #4667, #6489 ),
 ( #11646, #13456, #1450 ),
 ( #3400, #7160, #10479 ),
 ( #8435, #13681, #6952 ),
 ( #10255, #8879, #15405 ) ),
 .UNSPECIFIED., .F., .F., .F. ) 
 B_SPLINE_SURFACE_WITH_KNOTS ( ( 4, 2, 2, 2, 2, 2, 2, 2, 2, 2, 2, 2, 2, 2, 2, 4 ),
 ( 3, 3 ),
 ( 0.000000000000000000, 0.005810029919203039614, 0.008715044878804558554, 0.01162005983840607923, 0.01452507479800759817, 0.01743008975760911711, 0.02033510471721063778, 0.02324011967681215846, 0.02614513463641367913, 0.02905014959601519633, 0.03486017951521823421, 0.03631268699501899455, 0.03776519447481975489, 0.04067020943442127556, 0.04357522439402279624, 0.04648023935362431691 ),
 ( 0.000000000000000000, 1.000000000000000000 ),
 .UNSPECIFIED. ) 
 GEOMETRIC_REPRESENTATION_ITEM ( )  RATIONAL_B_SPLINE_SURFACE ( (
 ( 1.000000000000000000, 0.6428092274089118874, 1.000000000000000000),
 ( 1.000000000000000000, 0.6349692141176791482, 1.000000000000000000),
 ( 1.000000000000000000, 0.6297610438357627016, 1.000000000000000000),
 ( 1.000000000000000000, 0.6250724677584068578, 1.000000000000000000),
 ( 1.000000000000000000, 0.6240291009521158339, 1.000000000000000000),
 ( 1.000000000000000000, 0.6228114827670508946, 1.000000000000000000),
 ( 1.000000000000000000, 0.6226217323249613189, 1.000000000000000000),
 ( 1.000000000000000000, 0.6227877533346651839, 1.000000000000000000),
 ( 1.000000000000000000, 0.6231437405068817048, 1.000000000000000000),
 ( 1.000000000000000000, 0.6241327156851853575, 1.000000000000000000),
 ( 1.000000000000000000, 0.6247528374331501322, 1.000000000000000000),
 ( 1.000000000000000000, 0.6259854008234480016, 1.000000000000000000),
 ( 1.000000000000000000, 0.6265990906533466243, 1.000000000000000000),
 ( 1.000000000000000000, 0.6276348137172499397, 1.000000000000000000),
 ( 1.000000000000000000, 0.6280565648727459704, 1.000000000000000000),
 ( 1.000000000000000000, 0.6285705475697730416, 1.000000000000000000),
 ( 1.000000000000000000, 0.6286676444199297276, 1.000000000000000000),
 ( 1.000000000000000000, 0.6285219413518228215, 1.000000000000000000),
 ( 1.000000000000000000, 0.6282782847626313671, 1.000000000000000000),
 ( 1.000000000000000000, 0.6271139948532048480, 1.000000000000000000),
 ( 1.000000000000000000, 0.6257653971626693234, 1.000000000000000000),
 ( 1.000000000000000000, 0.6242767683748037255, 1.000000000000000000),
 ( 1.000000000000000000, 0.6239908339060202813, 1.000000000000000000),
 ( 1.000000000000000000, 0.6234800620765024171, 1.000000000000000000),
 ( 1.000000000000000000, 0.6232570855776793373, 1.000000000000000000),
 ( 1.000000000000000000, 0.6227348070543635705, 1.000000000000000000),
 ( 1.000000000000000000, 0.6225812994814358126, 1.000000000000000000),
 ( 1.000000000000000000, 0.6229454059004365662, 1.000000000000000000),
 ( 1.000000000000000000, 0.6234652178690811564, 1.000000000000000000),
 ( 1.000000000000000000, 0.6254772350196486919, 1.000000000000000000),
 ( 1.000000000000000000, 0.6269570472271859263, 1.000000000000000000),
 ( 1.000000000000000000, 0.6290213284793358950, 1.000000000000000000) ) ) 
 REPRESENTATION_ITEM ( '' )  SURFACE ( )  );
#4311 = ORIENTED_EDGE ( 'NONE', *, *, #5518, .F. ) ;
#4312 = LINE ( 'NONE', #19549, #17870 ) ;
#4313 = DIRECTION ( 'NONE',  ( -6.505213034913038160E-19, -3.903127820947822896E-18, -1.000000000000000000 ) ) ;
#4314 = ORIENTED_EDGE ( 'NONE', *, *, #16557, .F. ) ;
#4315 = EDGE_CURVE ( 'NONE', #19421, #728, #21506, .T. ) ;
#4316 = AXIS2_PLACEMENT_3D ( 'NONE', #18352, #3009, #13069 ) ;
#4317 = ORIENTED_EDGE ( 'NONE', *, *, #22598, .F. ) ;
#4318 = CARTESIAN_POINT ( 'NONE',  ( 2.220446049250313081E-13, -2.498001805406602216E-13, -6.859353255829918616 ) ) ;
#4319 = CIRCLE ( 'NONE', #8324, 17.00000000000001421 ) ;
#4320 = FACE_OUTER_BOUND ( 'NONE', #18037, .T. ) ;
#4321 = DIRECTION ( 'NONE',  ( -6.505213034913038160E-19, -3.903127820947822896E-18, -1.000000000000000000 ) ) ;
#4322 = CIRCLE ( 'NONE', #22253, 2.500000000000002220 ) ;
#4323 = ADVANCED_FACE ( 'NONE', ( #3818 ), #19854, .F. ) ;
#4324 = DIRECTION ( 'NONE',  ( -0.000000000000000000, -1.000000000000000000, -0.000000000000000000 ) ) ;
#4325 = AXIS2_PLACEMENT_3D ( 'NONE', #15578, #3789, #22601 ) ;
#4326 = CARTESIAN_POINT ( 'NONE',  ( 42.50000000000000711, -12.00000000000012434, 47.50000000000000711 ) ) ;
#4327 = ORIENTED_EDGE ( 'NONE', *, *, #16684, .F. ) ;
#4328 = CIRCLE ( 'NONE', #12724, 1.000000000000000888 ) ;
#4329 = ORIENTED_EDGE ( 'NONE', *, *, #650, .F. ) ;
#4330 = AXIS2_PLACEMENT_3D ( 'NONE', #7171, #3646, #20939 ) ;
#4331 = ORIENTED_EDGE ( 'NONE', *, *, #21833, .T. ) ;
#4332 = CARTESIAN_POINT ( 'NONE',  ( 0.000000000000000000, -25.00000000000000000, 11.99999999999985256 ) ) ;
#4333 = LINE ( 'NONE', #997, #6879 ) ;
#4334 = CARTESIAN_POINT ( 'NONE',  ( 1.145276119298441975, 0.005126887280125313681, -49.65522505679928855 ) ) ;
#4335 = ADVANCED_FACE ( 'NONE', ( #12954 ), #2848, .T. ) ;
#4336 = AXIS2_PLACEMENT_3D ( 'NONE', #20180, #18000, #19844 ) ;
#4337 = DIRECTION ( 'NONE',  ( 6.505213034913038160E-19, 3.903127820947822896E-18, 1.000000000000000000 ) ) ;
#4338 = DIRECTION ( 'NONE',  ( 6.505213034913038160E-19, 3.903127820947822896E-18, 1.000000000000000000 ) ) ;
#4339 = DIRECTION ( 'NONE',  ( 0.000000000000000000, 0.000000000000000000, -1.000000000000000000 ) ) ;
#4340 = CARTESIAN_POINT ( 'NONE',  ( 1.423424233832709662, 32.35999952201570551, -2.999999999999975131 ) ) ;
#4341 = DIRECTION ( 'NONE',  ( 0.000000000000000000, 0.000000000000000000, 1.000000000000000000 ) ) ;
#4342 = AXIS2_PLACEMENT_3D ( 'NONE', #21017, #9195, #16170 ) ;
#4343 = CIRCLE ( 'NONE', #8739, 1.000000000000000888 ) ;
#4344 = VERTEX_POINT ( 'NONE', #12840 ) ;
#4345 = EDGE_CURVE ( 'NONE', #18209, #22365, #13434, .T. ) ;
#4346 = AXIS2_PLACEMENT_3D ( 'NONE', #11743, #2939, #8530 ) ;
#4347 = CARTESIAN_POINT ( 'NONE',  ( 13.00000000000024336, -2.516660498395250745, -100.0000000000000000 ) ) ;
#4348 = CARTESIAN_POINT ( 'NONE',  ( -36.54278193890295512, -4.025500340002762911, -2.800654218530457484 ) ) ;
#4349 = CARTESIAN_POINT ( 'NONE',  ( 11.85401191286899980, 32.83234229683715455, 2.999999999999995559 ) ) ;
#4350 = CIRCLE ( 'NONE', #20817, 2.499999999999998668 ) ;
#4351 = VERTEX_POINT ( 'NONE', #4053 ) ;
#4352 = CARTESIAN_POINT ( 'NONE',  ( -14.30873905802322632, -28.06260833510309993, -2.999999999999957367 ) ) ;
#4353 = CARTESIAN_POINT ( 'NONE',  ( 90.00000000000000000, 40.00000000000000000, 2.099999999999989875 ) ) ;
#4354 = DIRECTION ( 'NONE',  ( 1.296372316667914327E-16, 1.000000000000000000, -0.000000000000000000 ) ) ;
#4355 = LINE ( 'NONE', #9843, #5362 ) ;
#4356 = EDGE_CURVE ( 'NONE', #8405, #10917, #16739, .T. ) ;
#4357 = AXIS2_PLACEMENT_3D ( 'NONE', #15647, #1338, #20483 ) ;
#4358 = AXIS2_PLACEMENT_3D ( 'NONE', #18098, #347, #4132 ) ;
#4359 = ORIENTED_EDGE ( 'NONE', *, *, #9254, .F. ) ;
#4360 = DIRECTION ( 'NONE',  ( -0.000000000000000000, -1.000000000000000000, -0.000000000000000000 ) ) ;
#4361 = ADVANCED_FACE ( 'NONE', ( #17786 ), #8962, .T. ) ;
#4362 = CARTESIAN_POINT ( 'NONE',  ( -4.104665049622623130, 35.91964150878174422, -2.933296326616367189 ) ) ;
#4363 = VERTEX_POINT ( 'NONE', #12498 ) ;
#4364 = CARTESIAN_POINT ( 'NONE',  ( 0.3359095670093927288, 39.99934629023403687, -48.99369681844596869 ) ) ;
#4365 = CARTESIAN_POINT ( 'NONE',  ( 35.00000000000001421, -1.000000000000028644, 1.540743955509788682E-30 ) ) ;
#4366 = FACE_OUTER_BOUND ( 'NONE', #20936, .T. ) ;
#4367 = DIRECTION ( 'NONE',  ( 0.000000000000000000, 0.000000000000000000, -1.000000000000000000 ) ) ;
#4368 = DIRECTION ( 'NONE',  ( 1.000000000000000000, 8.005695478557271943E-15, 0.000000000000000000 ) ) ;
#4369 = CARTESIAN_POINT ( 'NONE',  ( -2.777956037036614756, 39.99999999999999289, 50.42551054490269991 ) ) ;
#4370 = DIRECTION ( 'NONE',  ( -6.505213034913038160E-19, -3.903127820947822896E-18, -1.000000000000000000 ) ) ;
#4371 = TOROIDAL_SURFACE ( 'NONE', #17158, 22.00000000000000000, 2.000000000000000000 ) ;
#4372 = ORIENTED_EDGE ( 'NONE', *, *, #8821, .F. ) ;
#4373 = DIRECTION ( 'NONE',  ( -6.505213034913038160E-19, -3.903127820947822896E-18, -1.000000000000000000 ) ) ;
#4374 = CARTESIAN_POINT ( 'NONE',  ( -10.70799354677358295, 35.16985127952384715, -2.800654218530457484 ) ) ;
#4375 = CARTESIAN_POINT ( 'NONE',  ( -0.03435155977924175819, 39.99999305009784223, -48.76069593537407343 ) ) ;
#4376 = VERTEX_POINT ( 'NONE', #19627 ) ;
#4377 = CARTESIAN_POINT ( 'NONE',  ( -11.84669267190940722, 29.23061840495885733, 44.31876460048059840 ) ) ;
#4378 = DIRECTION ( 'NONE',  ( 0.000000000000000000, -1.000000000000000000, 0.000000000000000000 ) ) ;
#4379 = EDGE_CURVE ( 'NONE', #13224, #13528, #22248, .T. ) ;
#4380 = PRODUCT_DEFINITION_SHAPE ( 'NONE', 'NONE',  #17947 ) ;
#4381 = VERTEX_POINT ( 'NONE', #9191 ) ;
#4382 = EDGE_CURVE ( 'NONE', #21335, #16994, #6134, .T. ) ;
#4383 = AXIS2_PLACEMENT_3D ( 'NONE', #15739, #12089, #51 ) ;
#4384 = ORIENTED_EDGE ( 'NONE', *, *, #17438, .F. ) ;
#4385 = ORIENTED_EDGE ( 'NONE', *, *, #11163, .T. ) ;
#4386 = CARTESIAN_POINT ( 'NONE',  ( 11.09836907989742905, 40.00000000000000000, 54.00358115607141229 ) ) ;
#4387 = CARTESIAN_POINT ( 'NONE',  ( -34.99999999999998579, -3.999999999999985345, -59.99999999999703704 ) ) ;
#4388 = CARTESIAN_POINT ( 'NONE',  ( 24.73600648735135721, -27.19760187735878532, 2.800654218530481465 ) ) ;
#4389 = CARTESIAN_POINT ( 'NONE',  ( -34.99999999999980815, 26.00000000000000355, 52.89999999999922409 ) ) ;
#4390 = CARTESIAN_POINT ( 'NONE',  ( -5.011587927596626635, 5.833858253127846893, -40.02147800532274147 ) ) ;
#4391 = ORIENTED_EDGE ( 'NONE', *, *, #9058, .F. ) ;
#4392 = CARTESIAN_POINT ( 'NONE',  ( 3.071904583821672593E-15, -4.500000000000010658, 0.000000000000000000 ) ) ;
#4393 = CARTESIAN_POINT ( 'NONE',  ( 30.33632613426201630, -11.35354668330712613, 2.999999999999995559 ) ) ;
#4394 = ORIENTED_EDGE ( 'NONE', *, *, #17169, .F. ) ;
#4395 = CARTESIAN_POINT ( 'NONE',  ( -8.188149873056877581, 7.413691783916331879, -42.20917188641858075 ) ) ;
#4396 = CARTESIAN_POINT ( 'NONE',  ( -25.00000000000000000, 20.00000000000000000, 6.487780019669002523E-15 ) ) ;
#4397 = AXIS2_PLACEMENT_3D ( 'NONE', #15235, #13516, #18698 ) ;
#4398 = CARTESIAN_POINT ( 'NONE',  ( 1.570149971351546103, 40.00000000000000000, 49.72616472077324801 ) ) ;
#4399 = ORIENTED_EDGE ( 'NONE', *, *, #3759, .T. ) ;
#4400 = CARTESIAN_POINT ( 'NONE',  ( -1.387778780781445518E-14, 20.00000000000000355, 103.0000000000000284 ) ) ;
#4401 = EDGE_CURVE ( 'NONE', #4117, #17014, #19680, .T. ) ;
#4402 = CARTESIAN_POINT ( 'NONE',  ( 3.315551171824481003, 0.2472631163781295605, 51.08212483309238650 ) ) ;
#4403 = VERTEX_POINT ( 'NONE', #18462 ) ;
#4404 = CARTESIAN_POINT ( 'NONE',  ( 8.123071147678585291, 39.63120350560809868, 53.85470533195105958 ) ) ;
#4405 = CARTESIAN_POINT ( 'NONE',  ( 27.62019382530525391, -4.341204441673157888, -5.000000000000004441 ) ) ;
#4406 = ORIENTED_EDGE ( 'NONE', *, *, #9942, .T. ) ;
#4407 = UNCERTAINTY_MEASURE_WITH_UNIT (LENGTH_MEASURE( 1.000000000000000082E-05 ), #180, 'distance_accuracy_value', 'NONE');
#4408 = AXIS2_PLACEMENT_3D ( 'NONE', #21234, #14219, #12501 ) ;
#4409 = DIRECTION ( 'NONE',  ( 0.000000000000000000, 0.000000000000000000, -1.000000000000000000 ) ) ;
#4410 = DIRECTION ( 'NONE',  ( -1.000000000000000000, -4.975008120446308529E-14, 0.000000000000000000 ) ) ;
#4411 = EDGE_CURVE ( 'NONE', #13828, #11150, #1272, .T. ) ;
#4412 = DIRECTION ( 'NONE',  ( 8.659560562355083235E-17, 0.7071067811865352493, -0.7071067811865597852 ) ) ;
#4413 = CARTESIAN_POINT ( 'NONE',  ( 19.43475998741689281, 8.756352882854699260, -57.94642939675669169 ) ) ;
#4414 = VERTEX_POINT ( 'NONE', #1161 ) ;
#4415 = AXIS2_PLACEMENT_3D ( 'NONE', #10171, #3084, #22115 ) ;
#4416 = ORIENTED_EDGE ( 'NONE', *, *, #21182, .F. ) ;
#4417 = ORIENTED_EDGE ( 'NONE', *, *, #21829, .F. ) ;
#4418 = ORIENTED_EDGE ( 'NONE', *, *, #3492, .T. ) ;
#4419 = CARTESIAN_POINT ( 'NONE',  ( -14.14132741310371344, -16.85297774861763287, 2.999999999999995559 ) ) ;
#4420 = DIRECTION ( 'NONE',  ( 0.000000000000000000, 0.000000000000000000, 1.000000000000000000 ) ) ;
#4421 = VERTEX_POINT ( 'NONE', #6099 ) ;
#4422 = CYLINDRICAL_SURFACE ( 'NONE', #12020, 1.000000000000000888 ) ;
#4423 = CARTESIAN_POINT ( 'NONE',  ( -1.516119572518642933, 13.38525031373512064, 6.878942250887981835 ) ) ;
#4424 = ORIENTED_EDGE ( 'NONE', *, *, #18472, .F. ) ;
#4425 = CARTESIAN_POINT ( 'NONE',  ( 2.673152730111972630, 14.43024452475228614, 6.612623190900158043 ) ) ;
#4426 = EDGE_CURVE ( 'NONE', #8747, #14227, #18943, .T. ) ;
#4427 = ORIENTED_EDGE ( 'NONE', *, *, #18915, .T. ) ;
#4428 = LINE ( 'NONE', #20124, #18146 ) ;
#4429 = DIRECTION ( 'NONE',  ( 0.000000000000000000, 0.000000000000000000, 1.000000000000000000 ) ) ;
#4430 = DIRECTION ( 'NONE',  ( 0.000000000000000000, 0.000000000000000000, -1.000000000000000000 ) ) ;
#4431 = CARTESIAN_POINT ( 'NONE',  ( -1.387778780781445676E-14, 20.00000000000000000, -98.00000000000000000 ) ) ;
#4432 = CIRCLE ( 'NONE', #12824, 2.099999999999997868 ) ;
#4433 = EDGE_CURVE ( 'NONE', #11772, #6084, #7969, .T. ) ;
#4434 = EDGE_CURVE ( 'NONE', #18399, #11377, #3592, .T. ) ;
#4435 = EDGE_CURVE ( 'NONE', #17014, #18120, #22621, .T. ) ;
#4436 = CARTESIAN_POINT ( 'NONE',  ( -3.630529889112771524, 39.68566040249004345, 51.94953878410922954 ) ) ;
#4437 = DIRECTION ( 'NONE',  ( -1.000000000000000000, 1.264902534566421922E-16, 0.000000000000000000 ) ) ;
#4438 = ORIENTED_EDGE ( 'NONE', *, *, #17655, .F. ) ;
#4439 = VERTEX_POINT ( 'NONE', #16749 ) ;
#4440 = EDGE_CURVE ( 'NONE', #4746, #877, #19324, .T. ) ;
#4441 = ORIENTED_EDGE ( 'NONE', *, *, #1644, .F. ) ;
#4442 = CARTESIAN_POINT ( 'NONE',  ( -20.25803107563953631, 29.70716601075176300, 58.16264420749882191 ) ) ;
#4443 = DIRECTION ( 'NONE',  ( 1.000000000000000000, 0.000000000000000000, 0.000000000000000000 ) ) ;
#4444 = AXIS2_PLACEMENT_3D ( 'NONE', #1273, #6553, #13957 ) ;
#4445 = DIRECTION ( 'NONE',  ( 0.000000000000000000, 0.000000000000000000, 1.000000000000000000 ) ) ;
#4446 = DIRECTION ( 'NONE',  ( -1.000000000000000000, 1.084202172485504434E-16, 0.000000000000000000 ) ) ;
#4447 = DIRECTION ( 'NONE',  ( 0.000000000000000000, 0.000000000000000000, -1.000000000000000000 ) ) ;
#4448 = CARTESIAN_POINT ( 'NONE',  ( 2.775557561562891351E-14, -2.775557561562891351E-14, 2.999999999999999112 ) ) ;
#4449 = DIRECTION ( 'NONE',  ( 0.000000000000000000, 1.000000000000000000, 0.000000000000000000 ) ) ;
#4450 = CARTESIAN_POINT ( 'NONE',  ( -8.970854721945018539, 37.88903791882350447, -54.67446985351440958 ) ) ;
#4451 = CARTESIAN_POINT ( 'NONE',  ( 35.99819890246974552, -7.463862311151231665, 2.800654218530509443 ) ) ;
#4452 = CIRCLE ( 'NONE', #797, 2.499999999999995115 ) ;
#4453 = VECTOR ( 'NONE', #10143, 1000.000000000000114 ) ;
#4454 = ORIENTED_EDGE ( 'NONE', *, *, #893, .T. ) ;
#4455 = CARTESIAN_POINT ( 'NONE',  ( 42.50000000000000711, -5.000000000000000000, -49.60000000000000142 ) ) ;
#4456 = CARTESIAN_POINT ( 'NONE',  ( 34.99999999999980815, 28.00000000000000000, 54.99999999999922551 ) ) ;
#4457 = CARTESIAN_POINT ( 'NONE',  ( 14.31754202316508540, 5.927758996453707852, 58.94936959136226307 ) ) ;
#4458 = CYLINDRICAL_SURFACE ( 'NONE', #14761, 59.99999999999703704 ) ;
#4459 = EDGE_LOOP ( 'NONE', ( #11575, #5939, #8184, #6790, #21741, #20951 ) ) ;
#4460 = FACE_OUTER_BOUND ( 'NONE', #17382, .T. ) ;
#4461 = VERTEX_POINT ( 'NONE', #20422 ) ;
#4462 = CARTESIAN_POINT ( 'NONE',  ( -35.00000000000000000, -4.928932188134504955, 1.387778780781445676E-14 ) ) ;
#4463 = CARTESIAN_POINT ( 'NONE',  ( -35.00000000000000000, 0.000000000000000000, -40.99999999999997868 ) ) ;
#4464 = EDGE_CURVE ( 'NONE', #12113, #20626, #15765, .T. ) ;
#4465 = ADVANCED_FACE ( 'NONE', ( #4275 ), #14894, .F. ) ;
#4466 = ORIENTED_EDGE ( 'NONE', *, *, #2324, .T. ) ;
#4467 = LINE ( 'NONE', #4124, #7832 ) ;
#4468 = AXIS2_PLACEMENT_3D ( 'NONE', #808, #4370, #4477 ) ;
#4469 = EDGE_CURVE ( 'NONE', #5777, #16804, #2624, .T. ) ;
#4470 = DIRECTION ( 'NONE',  ( -1.000000000000000000, 1.815202222194848473E-15, 0.000000000000000000 ) ) ;
#4471 = ORIENTED_EDGE ( 'NONE', *, *, #5213, .T. ) ;
#4472 = CARTESIAN_POINT ( 'NONE',  ( 15.02862401740806497, 32.75570538720773328, -2.999999999999999112 ) ) ;
#4473 = DIRECTION ( 'NONE',  ( -1.000000000000000000, 0.000000000000000000, 0.000000000000000000 ) ) ;
#4474 = CYLINDRICAL_SURFACE ( 'NONE', #14916, 1.000000000000000888 ) ;
#4475 = DIRECTION ( 'NONE',  ( -0.000000000000000000, 1.000000000000000000, -0.000000000000000000 ) ) ;
#4476 = DIRECTION ( 'NONE',  ( 6.505213034913038160E-19, 3.903127820947822896E-18, 1.000000000000000000 ) ) ;
#4477 = DIRECTION ( 'NONE',  ( -1.000000000000000000, 0.000000000000000000, 0.000000000000000000 ) ) ;
#4478 = VERTEX_POINT ( 'NONE', #9643 ) ;
#4479 = DIRECTION ( 'NONE',  ( 0.000000000000000000, 0.000000000000000000, -1.000000000000000000 ) ) ;
#4480 = DIRECTION ( 'NONE',  ( 8.659560562353731078E-17, 0.7071067811866457165, -0.7071067811864494290 ) ) ;
#4481 = CARTESIAN_POINT ( 'NONE',  ( 42.50000000000000711, -12.00000000000000000, -41.00000000000000000 ) ) ;
#4482 = CARTESIAN_POINT ( 'NONE',  ( -0.01280385524457875075, 39.99999915041527743, -48.74393752659626955 ) ) ;
#4483 = ORIENTED_EDGE ( 'NONE', *, *, #19770, .T. ) ;
#4484 = CARTESIAN_POINT ( 'NONE',  ( -4.025500340002513333, 36.54278193890309012, -2.800654218530457484 ) ) ;
#4485 = EDGE_CURVE ( 'NONE', #12526, #1555, #22018, .T. ) ;
#4486 = AXIS2_PLACEMENT_3D ( 'NONE', #14247, #21262, #5553 ) ;
#4487 = DIRECTION ( 'NONE',  ( 1.000000000000000000, 1.208970125616053784E-17, 0.000000000000000000 ) ) ;
#4488 = DIRECTION ( 'NONE',  ( 0.000000000000000000, 0.000000000000000000, -1.000000000000000000 ) ) ;
#4489 = ORIENTED_EDGE ( 'NONE', *, *, #17376, .T. ) ;
#4490 = EDGE_LOOP ( 'NONE', ( #4871, #17342 ) ) ;
#4491 =( LENGTH_UNIT ( ) NAMED_UNIT ( * ) SI_UNIT ( .MILLI., .METRE. ) );
#4492 = ORIENTED_EDGE ( 'NONE', *, *, #9847, .T. ) ;
#4493 = CARTESIAN_POINT ( 'NONE',  ( 15.58352763714662892, 32.54529335663308132, 59.37339313163358412 ) ) ;
#4494 = DIRECTION ( 'NONE',  ( -6.505213034913038160E-19, -3.903127820947822896E-18, -1.000000000000000000 ) ) ;
#4495 = VECTOR ( 'NONE', #8025, 1000.000000000000000 ) ;
#4496 = CONICAL_SURFACE ( 'NONE', #9232, 2.525000000000110489, 0.7853981633971014453 ) ;
#4497 = CARTESIAN_POINT ( 'NONE',  ( -1.387778780781445518E-14, 20.00000000000000355, 103.0000000000000284 ) ) ;
#4498 = DIRECTION ( 'NONE',  ( 0.000000000000000000, 0.000000000000000000, 1.000000000000000000 ) ) ;
#4499 = DIRECTION ( 'NONE',  ( 0.000000000000000000, -1.000000000000000000, 0.000000000000000000 ) ) ;
#4500 = EDGE_LOOP ( 'NONE', ( #1973, #10839, #16806, #19862 ) ) ;
#4501 = DIRECTION ( 'NONE',  ( 1.000000000000000000, 1.208970125616053475E-17, 0.000000000000000000 ) ) ;
#4502 = CARTESIAN_POINT ( 'NONE',  ( 32.10132595304146719, 5.074925817841635656, 2.999999999999995559 ) ) ;
#4503 = EDGE_LOOP ( 'NONE', ( #16138, #13930, #14702, #3407 ) ) ;
#4504 = DIRECTION ( 'NONE',  ( 6.505213034913038160E-19, 3.903127820947822896E-18, 1.000000000000000000 ) ) ;
#4505 = AXIS2_PLACEMENT_3D ( 'NONE', #1667, #10584, #21030 ) ;
#4506 = EDGE_CURVE ( 'NONE', #817, #4626, #1880, .T. ) ;
#4507 = CARTESIAN_POINT ( 'NONE',  ( -18.49252681899431039, 7.260825773989761700, -57.68517796515786245 ) ) ;
#4508 = DIRECTION ( 'NONE',  ( -1.000000000000000000, 0.000000000000000000, 0.000000000000000000 ) ) ;
#4509 = CARTESIAN_POINT ( 'NONE',  ( 11.35354668330723626, 30.33632613426176405, 2.999999999999999112 ) ) ;
#4510 = ORIENTED_EDGE ( 'NONE', *, *, #22195, .F. ) ;
#4511 = DIRECTION ( 'NONE',  ( 1.000000000000000000, 0.000000000000000000, 0.000000000000000000 ) ) ;
#4512 = CARTESIAN_POINT ( 'NONE',  ( -16.66666666666665719, 20.00000000000000000, 23.57022603955159923 ) ) ;
#4513 = ORIENTED_EDGE ( 'NONE', *, *, #2005, .T. ) ;
#4514 = DIRECTION ( 'NONE',  ( -0.000000000000000000, 1.000000000000000000, -0.000000000000000000 ) ) ;
#4515 =( NAMED_UNIT ( * ) SI_UNIT ( $, .STERADIAN. ) SOLID_ANGLE_UNIT ( ) );
#4516 = EDGE_CURVE ( 'NONE', #5200, #16687, #22138, .T. ) ;
#4517 = ORIENTED_EDGE ( 'NONE', *, *, #11352, .F. ) ;
#4518 = ADVANCED_FACE ( 'NONE', ( #18696 ), #22170, .T. ) ;
#4519 = CARTESIAN_POINT ( 'NONE',  ( 10.88890858922251326, 36.78121034548748014, 57.56873443369040189 ) ) ;
#4520 = CYLINDRICAL_SURFACE ( 'NONE', #9268, 2.500000000000002220 ) ;
#4521 = CIRCLE ( 'NONE', #6705, 17.00000000000000711 ) ;
#4522 = CARTESIAN_POINT ( 'NONE',  ( 18.69481036107318417, 7.531781294123580217, -57.74428367179856281 ) ) ;
#4523 = AXIS2_PLACEMENT_3D ( 'NONE', #270, #14233, #17920 ) ;
#4524 = CONICAL_SURFACE ( 'NONE', #5254, 18.00000000000000000, 0.7853981633974540522 ) ;
#4525 = ORIENTED_EDGE ( 'NONE', *, *, #18092, .T. ) ;
#4526 = ORIENTED_EDGE ( 'NONE', *, *, #2470, .F. ) ;
#4527 = EDGE_CURVE ( 'NONE', #11599, #11128, #5194, .T. ) ;
#4528 = ORIENTED_EDGE ( 'NONE', *, *, #18625, .F. ) ;
#4529 = ORIENTED_EDGE ( 'NONE', *, *, #9755, .F. ) ;
#4530 = CYLINDRICAL_SURFACE ( 'NONE', #7774, 1.000000000000001776 ) ;
#4531 = DIRECTION ( 'NONE',  ( -6.505213034913038160E-19, -3.903127820947822896E-18, -1.000000000000000000 ) ) ;
#4532 = AXIS2_PLACEMENT_3D ( 'NONE', #2953, #9927, #1456 ) ;
#4533 = ORIENTED_EDGE ( 'NONE', *, *, #20797, .T. ) ;
#4534 = DIRECTION ( 'NONE',  ( -0.000000000000000000, 1.000000000000000000, -0.000000000000000000 ) ) ;
#4535 = DIRECTION ( 'NONE',  ( 6.505213034913038160E-19, 3.903127820947822896E-18, 1.000000000000000000 ) ) ;
#4536 = ORIENTED_EDGE ( 'NONE', *, *, #22202, .F. ) ;
#4537 = EDGE_CURVE ( 'NONE', #349, #4006, #12258, .T. ) ;
#4538 = CARTESIAN_POINT ( 'NONE',  ( -0.7921581640248792633, 13.00083933661134417, 8.999720221269573273 ) ) ;
#4539 = AXIS2_PLACEMENT_3D ( 'NONE', #8996, #21607, #288 ) ;
#4540 = ORIENTED_EDGE ( 'NONE', *, *, #11064, .T. ) ;
#4541 = DIRECTION ( 'NONE',  ( 6.505213034913038160E-19, 3.903127820947822896E-18, 1.000000000000000000 ) ) ;
#4542 = CIRCLE ( 'NONE', #9283, 14.00000000000000000 ) ;
#4543 = DIRECTION ( 'NONE',  ( 0.000000000000000000, 1.000000000000000000, 0.000000000000000000 ) ) ;
#4544 = DIRECTION ( 'NONE',  ( -1.000000000000000000, 0.000000000000000000, 0.000000000000000000 ) ) ;
#4545 = CARTESIAN_POINT ( 'NONE',  ( -14.32898074910540842, 33.98521869245691107, -58.94425321795623063 ) ) ;
#4546 = AXIS2_PLACEMENT_3D ( 'NONE', #3898, #12362, #5385 ) ;
#4547 = EDGE_CURVE ( 'NONE', #13043, #9609, #8486, .T. ) ;
#4548 = AXIS2_PLACEMENT_3D ( 'NONE', #988, #13222, #16801 ) ;
#4549 = CARTESIAN_POINT ( 'NONE',  ( 28.96193690644943786, 14.74639653023224284, -2.999999999999971578 ) ) ;
#4550 = ORIENTED_EDGE ( 'NONE', *, *, #20384, .F. ) ;
#4551 = AXIS2_PLACEMENT_3D ( 'NONE', #5699, #537, #14507 ) ;
#4552 = ORIENTED_EDGE ( 'NONE', *, *, #13457, .F. ) ;
#4553 = EDGE_CURVE ( 'NONE', #17173, #4794, #6860, .T. ) ;
#4554 = ORIENTED_EDGE ( 'NONE', *, *, #5776, .T. ) ;
#4555 = CARTESIAN_POINT ( 'NONE',  ( -17.83526554138388676, 10.93913794110440207, 60.06225905488084749 ) ) ;
#4556 = CARTESIAN_POINT ( 'NONE',  ( -30.48934413892778750, 16.99647590252656570, 2.999999999999999112 ) ) ;
#4557 = CARTESIAN_POINT ( 'NONE',  ( -31.57187188083528184, -7.711478842616553919, 3.000000000000023537 ) ) ;
#4558 = DIRECTION ( 'NONE',  ( 0.000000000000000000, 0.000000000000000000, 1.000000000000000000 ) ) ;
#4559 = ADVANCED_FACE ( 'NONE', ( #20529 ), #1615, .F. ) ;
#4560 = FACE_OUTER_BOUND ( 'NONE', #18214, .T. ) ;
#4561 = CIRCLE ( 'NONE', #20298, 0.9999999999999995559 ) ;
#4562 = CARTESIAN_POINT ( 'NONE',  ( -25.00000000000000000, 20.00000000000000000, 6.487780019669002523E-15 ) ) ;
#4563 = B_SPLINE_CURVE_WITH_KNOTS ( 'NONE', 3,
 ( #3022, #13418, #3251, #16983 ),
 .UNSPECIFIED., .F., .F.,
 ( 4, 4 ),
 ( 0.001875451646902537165, 0.003761979286330901194 ),
 .UNSPECIFIED. ) ;
#4564 = CYLINDRICAL_SURFACE ( 'NONE', #9751, 2.499999999999995115 ) ;
#4565 = CARTESIAN_POINT ( 'NONE',  ( 3.330669073875469621E-13, -1.110223024625156540E-13, -2.999999999999971578 ) ) ;
#4566 = CARTESIAN_POINT ( 'NONE',  ( 4.084299015952138845, -4.682619376883142337, 48.27507093818913120 ) ) ;
#4567 = CARTESIAN_POINT ( 'NONE',  ( -35.00000000000000000, 38.99999999999999289, 1.387778780781445676E-14 ) ) ;
#4568 = ORIENTED_EDGE ( 'NONE', *, *, #20919, .T. ) ;
#4569 = FACE_OUTER_BOUND ( 'NONE', #8724, .T. ) ;
#4570 = EDGE_CURVE ( 'NONE', #10093, #17988, #8770, .T. ) ;
#4571 = DIRECTION ( 'NONE',  ( -0.000000000000000000, -1.000000000000000000, -0.000000000000000000 ) ) ;
#4572 = CARTESIAN_POINT ( 'NONE',  ( 13.06496334681581395, 4.761428254737779753, 58.49034434780526936 ) ) ;
#4573 = CARTESIAN_POINT ( 'NONE',  ( -26.00000000000001421, 19.99999999999982947, -100.0000000000000000 ) ) ;
#4574 = VECTOR ( 'NONE', #1750, 1000.000000000000000 ) ;
#4575 = EDGE_LOOP ( 'NONE', ( #2774, #6353 ) ) ;
#4576 = FACE_OUTER_BOUND ( 'NONE', #16265, .T. ) ;
#4577 = CARTESIAN_POINT ( 'NONE',  ( -35.16985127952396084, -10.70799354677381920, -1.999999999999977573 ) ) ;
#4578 = CARTESIAN_POINT ( 'NONE',  ( 34.09574698892499356, 10.01544929272282580, 3.000000000000049294 ) ) ;
#4579 = EDGE_CURVE ( 'NONE', #13430, #14737, #15040, .T. ) ;
#4580 = EDGE_CURVE ( 'NONE', #5486, #5841, #20871, .T. ) ;
#4581 = AXIS2_PLACEMENT_3D ( 'NONE', #17378, #5147, #8679 ) ;
#4582 = CYLINDRICAL_SURFACE ( 'NONE', #4905, 41.00000000000000000 ) ;
#4583 = CARTESIAN_POINT ( 'NONE',  ( 2.580936905856439978, 40.00000000000000711, -50.31086268949886176 ) ) ;
#4584 = VERTEX_POINT ( 'NONE', #17075 ) ;
#4585 = CARTESIAN_POINT ( 'NONE',  ( 36.39375341857542878, 7.980461308159686240, 2.999999999999995559 ) ) ;
#4586 = DIRECTION ( 'NONE',  ( 0.000000000000000000, 0.000000000000000000, 1.000000000000000000 ) ) ;
#4587 = CARTESIAN_POINT ( 'NONE',  ( 31.57187188083529605, 7.711478842616553919, -2.999999999999999112 ) ) ;
#4588 = AXIS2_PLACEMENT_3D ( 'NONE', #18485, #2801, #1081 ) ;
#4589 = CARTESIAN_POINT ( 'NONE',  ( 10.78076590486229058, 39.17366535989027199, -54.93576791445503460 ) ) ;
#4590 = EDGE_CURVE ( 'NONE', #4760, #11286, #21636, .T. ) ;
#4591 = LINE ( 'NONE', #8136, #15907 ) ;
#4592 = EDGE_CURVE ( 'NONE', #17027, #20227, #5906, .T. ) ;
#4593 = CARTESIAN_POINT ( 'NONE',  ( 7.463862311151453710, 35.99819890246924814, -1.999999999999977573 ) ) ;
#4594 = ORIENTED_EDGE ( 'NONE', *, *, #1472, .T. ) ;
#4595 = CARTESIAN_POINT ( 'NONE',  ( -34.13396246814566837, 14.93538271375399695, 2.999999999999995559 ) ) ;
#4596 = CARTESIAN_POINT ( 'NONE',  ( 7.577104390335129835, -0.4826542685317783410, 53.01683071947729076 ) ) ;
#4597 = CARTESIAN_POINT ( 'NONE',  ( 12.10743492718046532, 1.299801688895073637, -55.43551573823121004 ) ) ;
#4598 = DIRECTION ( 'NONE',  ( -0.000000000000000000, 1.000000000000000000, -0.000000000000000000 ) ) ;
#4599 = CIRCLE ( 'NONE', #562, 3.999999999999996447 ) ;
#4600 = ORIENTED_EDGE ( 'NONE', *, *, #13929, .F. ) ;
#4601 = ADVANCED_FACE ( 'NONE', ( #20754 ), #22040, .F. ) ;
#4602 = CARTESIAN_POINT ( 'NONE',  ( 1.734723475976807094E-14, -20.00000000000000000, 70.71067811865476926 ) ) ;
#4603 = CARTESIAN_POINT ( 'NONE',  ( 3.330669073875469621E-13, -1.110223024625156540E-13, -2.999999999999971578 ) ) ;
#4604 = AXIS2_PLACEMENT_3D ( 'NONE', #11825, #4963, #18944 ) ;
#4605 = VERTEX_POINT ( 'NONE', #12896 ) ;
#4606 = AXIS2_PLACEMENT_3D ( 'NONE', #17348, #8424, #15393 ) ;
#4607 = ORIENTED_EDGE ( 'NONE', *, *, #12288, .F. ) ;
#4608 = AXIS2_PLACEMENT_3D ( 'NONE', #147, #7142, #7375 ) ;
#4609 = DIRECTION ( 'NONE',  ( -0.003596745190944717653, -0.001882447320459817953, 0.9999917598741087099 ) ) ;
#4610 = ORIENTED_EDGE ( 'NONE', *, *, #7575, .T. ) ;
#4611 = CARTESIAN_POINT ( 'NONE',  ( 18.31820558117432896, 28.04217374067966162, 60.19578215372065699 ) ) ;
#4612 = AXIS2_PLACEMENT_3D ( 'NONE', #22677, #12218, #17146 ) ;
#4613 = DIRECTION ( 'NONE',  ( -0.000000000000000000, 1.000000000000000000, -0.000000000000000000 ) ) ;
#4614 = CARTESIAN_POINT ( 'NONE',  ( 0.000000000000000000, 1.500000000000015099, 19.99999999999999645 ) ) ;
#4615 = CARTESIAN_POINT ( 'NONE',  ( 11.68090480754630178, 3.765577839755386069, 57.90797000640142045 ) ) ;
#4616 = CARTESIAN_POINT ( 'NONE',  ( -35.00000000000000000, 2.142135623730931471, -59.99999999999998579 ) ) ;
#4617 = VERTEX_POINT ( 'NONE', #2615 ) ;
#4618 = DIRECTION ( 'NONE',  ( 0.000000000000000000, -1.000000000000000000, 0.000000000000000000 ) ) ;
#4619 = CARTESIAN_POINT ( 'NONE',  ( 35.00000000000001421, 5.000000000000000000, 9.000000000000035527 ) ) ;
#4620 = ORIENTED_EDGE ( 'NONE', *, *, #20136, .F. ) ;
#4621 = CARTESIAN_POINT ( 'NONE',  ( -14.98515767422211198, 19.22844023086510745, -45.81928800960655224 ) ) ;
#4622 = EDGE_CURVE ( 'NONE', #8683, #5161, #12467, .T. ) ;
#4623 = CARTESIAN_POINT ( 'NONE',  ( -32.09841355225989901, 5.093313992686310243, -2.999999999999971578 ) ) ;
#4624 = DIRECTION ( 'NONE',  ( -0.000000000000000000, -1.000000000000000000, -0.000000000000000000 ) ) ;
#4625 = CARTESIAN_POINT ( 'NONE',  ( 12.30135915900896215, 4.212003844039729827, -58.16904039079300759 ) ) ;
#4626 = VERTEX_POINT ( 'NONE', #11420 ) ;
#4627 = DIRECTION ( 'NONE',  ( -1.000000000000000000, 0.000000000000000000, 0.000000000000000000 ) ) ;
#4628 = CYLINDRICAL_SURFACE ( 'NONE', #7641, 0.9999999999999974465 ) ;
#4629 = ORIENTED_EDGE ( 'NONE', *, *, #930, .F. ) ;
#4630 = CARTESIAN_POINT ( 'NONE',  ( 48.93401015228426587, 7.000000000000000000, 46.57614213197968667 ) ) ;
#4631 = AXIS2_PLACEMENT_3D ( 'NONE', #5212, #15732, #8761 ) ;
#4632 = CARTESIAN_POINT ( 'NONE',  ( -7.545322633886957675, -0.4933377206467728926, -52.99899216500660515 ) ) ;
#4633 = AXIS2_PLACEMENT_3D ( 'NONE', #13899, #15504, #17117 ) ;
#4634 = ORIENTED_EDGE ( 'NONE', *, *, #16184, .T. ) ;
#4635 = CARTESIAN_POINT ( 'NONE',  ( 19.99999999999998579, 20.00000000000000355, 60.00200000000000244 ) ) ;
#4636 = EDGE_CURVE ( 'NONE', #8959, #5811, #14744, .T. ) ;
#4637 = CARTESIAN_POINT ( 'NONE',  ( -1.387778780781445518E-14, 20.00000000000000355, 105.0000000000000142 ) ) ;
#4638 = PLANE ( 'NONE',  #21326 ) ;
#4639 = CARTESIAN_POINT ( 'NONE',  ( 18.34034842040247426, 28.02508533842880212, -60.20240101109772723 ) ) ;
#4641 = EDGE_LOOP ( 'NONE', ( #15439, #20247, #4886, #22099 ) ) ;
#4640 = EDGE_CURVE ( 'NONE', #15853, #12856, #2726, .T. ) ;
#4642 = ORIENTED_EDGE ( 'NONE', *, *, #22627, .T. ) ;
#4643 = VERTEX_POINT ( 'NONE', #16229 ) ;
#4644 = AXIS2_PLACEMENT_3D ( 'NONE', #5773, #2333, #14584 ) ;
#4645 = ORIENTED_EDGE ( 'NONE', *, *, #10715, .T. ) ;
#4646 = FACE_OUTER_BOUND ( 'NONE', #14126, .T. ) ;
#4647 = CARTESIAN_POINT ( 'NONE',  ( 0.000000000000000000, 28.49999999999998934, -8.999999999999998224 ) ) ;
#4648 = EDGE_CURVE ( 'NONE', #12070, #5859, #13205, .T. ) ;
#4649 = ORIENTED_EDGE ( 'NONE', *, *, #21516, .T. ) ;
#4650 = DIRECTION ( 'NONE',  ( 0.000000000000000000, 1.000000000000000000, 0.000000000000000000 ) ) ;
#4651 = CARTESIAN_POINT ( 'NONE',  ( -7.682546357470768861, -2.941798577935520687, -52.37062424970645225 ) ) ;
#4652 = ORIENTED_EDGE ( 'NONE', *, *, #3921, .F. ) ;
#4653 = PLANE ( 'NONE',  #6608 ) ;
#4654 = CONICAL_SURFACE ( 'NONE', #7559, 19.99999999999999289, 1.308996938995746984 ) ;
#4655 = DIRECTION ( 'NONE',  ( 0.000000000000000000, 0.000000000000000000, -1.000000000000000000 ) ) ;
#4656 = ORIENTED_EDGE ( 'NONE', *, *, #1484, .F. ) ;
#4657 = CARTESIAN_POINT ( 'NONE',  ( 5.999999999999998224, -20.00000000000000000, -5.999999999999999112 ) ) ;
#4658 = DIRECTION ( 'NONE',  ( -0.000000000000000000, -1.000000000000000000, -0.000000000000000000 ) ) ;
#4659 = CARTESIAN_POINT ( 'NONE',  ( 1.325309500316239511E-14, -1.568768580316543204, -48.07879409069925458 ) ) ;
#4660 = DIRECTION ( 'NONE',  ( -1.000000000000000000, 0.000000000000000000, 0.000000000000000000 ) ) ;
#4661 = AXIS2_PLACEMENT_3D ( 'NONE', #20065, #7917, #7686 ) ;
#4662 = CARTESIAN_POINT ( 'NONE',  ( 1.734723475976807094E-14, -20.00000000000000000, 70.71067811865476926 ) ) ;
#4663 = EDGE_CURVE ( 'NONE', #10478, #10048, #2179, .T. ) ;
#4664 = ORIENTED_EDGE ( 'NONE', *, *, #7731, .F. ) ;
#4665 = EDGE_LOOP ( 'NONE', ( #8035, #2027, #11749, #12833 ) ) ;
#4666 = ORIENTED_EDGE ( 'NONE', *, *, #15942, .T. ) ;
#4667 = CARTESIAN_POINT ( 'NONE',  ( -15.23870778338556775, 7.010517948056213200, 56.68442755504044328 ) ) ;
#4668 = EDGE_CURVE ( 'NONE', #18864, #7376, #11750, .T. ) ;
#4669 = LINE ( 'NONE', #6490, #12538 ) ;
#4670 = AXIS2_PLACEMENT_3D ( 'NONE', #2784, #11811, #16970 ) ;
#4671 = AXIS2_PLACEMENT_3D ( 'NONE', #20316, #4504, #1281 ) ;
#4672 = CYLINDRICAL_SURFACE ( 'NONE', #13825, 36.76383501243555685 ) ;
#4673 = DIRECTION ( 'NONE',  ( -0.000000000000000000, -1.000000000000000000, -0.000000000000000000 ) ) ;
#4674 = AXIS2_PLACEMENT_3D ( 'NONE', #3323, #8236, #22343 ) ;
#4675 = CARTESIAN_POINT ( 'NONE',  ( -35.00000000000000000, 15.00000000000000000, -40.99999999999997868 ) ) ;
#4676 = ORIENTED_EDGE ( 'NONE', *, *, #3401, .F. ) ;
#4677 = LINE ( 'NONE', #19834, #8370 ) ;
#4678 = CARTESIAN_POINT ( 'NONE',  ( -32.09841355225970005, 5.093313992686226754, 2.999999999999995559 ) ) ;
#4679 = CARTESIAN_POINT ( 'NONE',  ( 31.67162468656012209, 14.67611967928900185, 3.000000000000002665 ) ) ;
#4680 = DIRECTION ( 'NONE',  ( -6.505213034913038160E-19, -3.903127820947822896E-18, -1.000000000000000000 ) ) ;
#4681 = CYLINDRICAL_SURFACE ( 'NONE', #11906, 4.999999999999997335 ) ;
#4682 = ADVANCED_FACE ( 'NONE', ( #6273 ), #16811, .T. ) ;
#4683 = ORIENTED_EDGE ( 'NONE', *, *, #13505, .T. ) ;
#4684 = LINE ( 'NONE', #4795, #4030 ) ;
#4685 = CARTESIAN_POINT ( 'NONE',  ( -42.50000000000000711, -12.00000000000000000, -47.50000000000000000 ) ) ;
#4686 = ORIENTED_EDGE ( 'NONE', *, *, #11357, .T. ) ;
#4687 = AXIS2_PLACEMENT_3D ( 'NONE', #18782, #10056, #5042 ) ;
#4688 = CARTESIAN_POINT ( 'NONE',  ( 6.696867368503558448E-15, 40.00000000000000000, 48.73397172404481381 ) ) ;
#4689 = DIRECTION ( 'NONE',  ( 0.000000000000000000, 1.000000000000000000, 0.000000000000000000 ) ) ;
#4690 = AXIS2_PLACEMENT_3D ( 'NONE', #4791, #17367, #15527 ) ;
#4691 = CARTESIAN_POINT ( 'NONE',  ( 15.02862401740828702, 32.75570538720756986, -6.999999999999950262 ) ) ;
#4692 = ADVANCED_FACE ( 'NONE', ( #14957 ), #17607, .T. ) ;
#4693 = EDGE_CURVE ( 'NONE', #19784, #14544, #14297, .T. ) ;
#4694 = AXIS2_PLACEMENT_3D ( 'NONE', #12344, #19355, #3661 ) ;
#4695 = EDGE_LOOP ( 'NONE', ( #17693, #20869, #7283, #1582 ) ) ;
#4696 = EDGE_LOOP ( 'NONE', ( #14995, #20897, #432, #14474 ) ) ;
#4697 = DIRECTION ( 'NONE',  ( 0.000000000000000000, 0.000000000000000000, -1.000000000000000000 ) ) ;
#4698 = VECTOR ( 'NONE', #4823, 1000.000000000000000 ) ;
#4699 = DIRECTION ( 'NONE',  ( 6.505213034913038160E-19, 3.903127820947822896E-18, 1.000000000000000000 ) ) ;
#4700 = VERTEX_POINT ( 'NONE', #20369 ) ;
#4701 = CIRCLE ( 'NONE', #17494, 19.11328065563152379 ) ;
#4702 = VECTOR ( 'NONE', #426, 1000.000000000000000 ) ;
#4703 = CYLINDRICAL_SURFACE ( 'NONE', #8427, 19.11328065563150957 ) ;
#4704 = AXIS2_PLACEMENT_3D ( 'NONE', #8446, #5352, #8891 ) ;
#4705 = DIRECTION ( 'NONE',  ( -6.505213034913038160E-19, -3.903127820947822896E-18, -1.000000000000000000 ) ) ;
#4706 = DIRECTION ( 'NONE',  ( 0.000000000000000000, 0.000000000000000000, 1.000000000000000000 ) ) ;
#4707 = DIRECTION ( 'NONE',  ( -0.000000000000000000, -0.000000000000000000, -1.000000000000000000 ) ) ;
#4708 = AXIS2_PLACEMENT_3D ( 'NONE', #3296, #8547, #13459 ) ;
#4709 = CARTESIAN_POINT ( 'NONE',  ( -13.76792553423404541, 26.00189441538237745, -45.26963775109936705 ) ) ;
#4710 = CARTESIAN_POINT ( 'NONE',  ( -10.49999999999980460, -2.516660498395515866, 60.00099999999999767 ) ) ;
#4711 = EDGE_CURVE ( 'NONE', #8574, #668, #9822, .T. ) ;
#4712 = ORIENTED_EDGE ( 'NONE', *, *, #21402, .T. ) ;
#4713 = FACE_OUTER_BOUND ( 'NONE', #20639, .T. ) ;
#4714 = CARTESIAN_POINT ( 'NONE',  ( -4.295527433237782828E-15, -1.236374842841486021, 48.24164917503448180 ) ) ;
#4715 = CARTESIAN_POINT ( 'NONE',  ( -34.99999999999999289, 0.000000000000000000, -52.49999999999705125 ) ) ;
#4716 = CARTESIAN_POINT ( 'NONE',  ( 35.00000000000000000, -15.00000000000000000, 2.255140518769849223E-14 ) ) ;
#4717 = ORIENTED_EDGE ( 'NONE', *, *, #621, .F. ) ;
#4718 = VECTOR ( 'NONE', #12540, 1000.000000000000000 ) ;
#4719 = CARTESIAN_POINT ( 'NONE',  ( -6.955395936296827841, -34.84717828836198805, -2.999999999999982236 ) ) ;
#4720 = CIRCLE ( 'NONE', #18620, 33.99999999999999289 ) ;
#4721 = ADVANCED_FACE ( 'NONE', ( #15064 ), #13564, .F. ) ;
#4722 = ADVANCED_FACE ( 'NONE', ( #13342 ), #18649, .F. ) ;
#4723 = EDGE_CURVE ( 'NONE', #1751, #15249, #20264, .T. ) ;
#4724 = AXIS2_PLACEMENT_3D ( 'NONE', #6114, #2331, #13076 ) ;
#4725 = AXIS2_PLACEMENT_3D ( 'NONE', #18838, #6582, #19064 ) ;
#4727 = ADVANCED_FACE ( 'NONE', ( #3179 ), #15176, .F. ) ;
#4726 = ORIENTED_EDGE ( 'NONE', *, *, #13705, .F. ) ;
#4728 = EDGE_CURVE ( 'NONE', #6038, #7926, #6526, .T. ) ;
#4729 = ORIENTED_EDGE ( 'NONE', *, *, #3652, .T. ) ;
#4730 = ITEM_DEFINED_TRANSFORMATION ( 'NONE', 'NONE', #9849,  #18273 ) ;
#4731 = ORIENTED_EDGE ( 'NONE', *, *, #11521, .F. ) ;
#4732 = CARTESIAN_POINT ( 'NONE',  ( 18.87121696173697316, 26.69448804128720809, -60.34297443853446197 ) ) ;
#4733 = CARTESIAN_POINT ( 'NONE',  ( -13.33780792070361443, 2.142135623730931471, 45.06383732350886362 ) ) ;
#4734 = LINE ( 'NONE', #20423, #6260 ) ;
#4735 = CARTESIAN_POINT ( 'NONE',  ( -9.708269511265271490, 33.52953626616022831, 2.999999999999999112 ) ) ;
#4736 = AXIS2_PLACEMENT_3D ( 'NONE', #14611, #21727, #525 ) ;
#4737 = DIRECTION ( 'NONE',  ( -0.000000000000000000, 1.000000000000000000, -0.000000000000000000 ) ) ;
#4738 = ORIENTED_EDGE ( 'NONE', *, *, #6654, .T. ) ;
#4739 = CARTESIAN_POINT ( 'NONE',  ( -34.99999999999999289, 5.000000000000000000, -3.012171160963566127E-14 ) ) ;
#4740 = CIRCLE ( 'NONE', #20468, 20.00000000000002132 ) ;
#4741 = EDGE_LOOP ( 'NONE', ( #1552, #1747, #1516, #16833, #19996 ) ) ;
#4742 = DIRECTION ( 'NONE',  ( -6.505213034913038160E-19, -3.903127820947822896E-18, -1.000000000000000000 ) ) ;
#4743 = DIRECTION ( 'NONE',  ( 0.000000000000000000, 1.000000000000000000, 0.000000000000000000 ) ) ;
#4744 = FACE_OUTER_BOUND ( 'NONE', #10514, .T. ) ;
#4745 = CARTESIAN_POINT ( 'NONE',  ( 9.728382623732244383, 39.99999999999997868, 53.57939893017088195 ) ) ;
#4746 = VERTEX_POINT ( 'NONE', #10945 ) ;
#4747 = CARTESIAN_POINT ( 'NONE',  ( -7.766911017765431247, 39.99999999999999289, -52.87044927329080934 ) ) ;
#4748 = ORIENTED_EDGE ( 'NONE', *, *, #2371, .T. ) ;
#4749 = CARTESIAN_POINT ( 'NONE',  ( 42.49999999999998579, 10.00000000000000000, -49.99999999999997868 ) ) ;
#4750 = CARTESIAN_POINT ( 'NONE',  ( 35.00000000000000000, 15.00000000000000000, 41.00000000000002132 ) ) ;
#4751 = ORIENTED_EDGE ( 'NONE', *, *, #11528, .T. ) ;
#4752 = DIRECTION ( 'NONE',  ( -0.000000000000000000, -1.000000000000000000, -0.000000000000000000 ) ) ;
#4753 = CARTESIAN_POINT ( 'NONE',  ( 34.99999999999980815, 40.00000000000000000, 57.09999999999921982 ) ) ;
#4754 = CARTESIAN_POINT ( 'NONE',  ( -6.000000000000000000, 20.00000000000000000, -5.999999999999999112 ) ) ;
#4755 = CARTESIAN_POINT ( 'NONE',  ( 19.45266119884270495, 15.02268094490047368, -60.49039575453066675 ) ) ;
#4757 = EDGE_CURVE ( 'NONE', #3371, #18887, #17318, .T. ) ;
#4756 = EDGE_LOOP ( 'NONE', ( #6381, #1486, #17696, #9217 ) ) ;
#4758 = EDGE_CURVE ( 'NONE', #19446, #19435, #2330, .T. ) ;
#4759 = VERTEX_POINT ( 'NONE', #18278 ) ;
#4760 = VERTEX_POINT ( 'NONE', #9467 ) ;
#4761 = ORIENTED_EDGE ( 'NONE', *, *, #18998, .F. ) ;
#4762 = CARTESIAN_POINT ( 'NONE',  ( -5.093313992686115732, -32.09841355226039639, -7.000000000000006217 ) ) ;
#4763 = CARTESIAN_POINT ( 'NONE',  ( 14.99999999999998579, 20.00000000000000000, 45.82575694955838230 ) ) ;
#4764 = EDGE_CURVE ( 'NONE', #2374, #21198, #6137, .T. ) ;
#4765 = VERTEX_POINT ( 'NONE', #17938 ) ;
#4766 = DIRECTION ( 'NONE',  ( 0.000000000000000000, 0.000000000000000000, 1.000000000000000000 ) ) ;
#4767 = CARTESIAN_POINT ( 'NONE',  ( 2.842671867368132155, 15.02807304850658987, 6.539645084689668764 ) ) ;
#4768 = VERTEX_POINT ( 'NONE', #7398 ) ;
#4769 = CARTESIAN_POINT ( 'NONE',  ( 2.775557561562891351E-14, -2.775557561562891351E-14, 2.999999999999995559 ) ) ;
#4770 = AXIS2_PLACEMENT_3D ( 'NONE', #15418, #4571, #1125 ) ;
#4771 = ORIENTED_EDGE ( 'NONE', *, *, #3851, .F. ) ;
#4772 = CARTESIAN_POINT ( 'NONE',  ( 90.00000000000000000, 26.00000000000000355, -9.108981535246192915E-16 ) ) ;
#4773 = CARTESIAN_POINT ( 'NONE',  ( 42.50000000000000711, -5.000000000000000000, 47.50000000000000711 ) ) ;
#4774 = CARTESIAN_POINT ( 'NONE',  ( -27.95348479018558763, 14.76298474240492276, 3.000000000000023537 ) ) ;
#4775 = CARTESIAN_POINT ( 'NONE',  ( -19.64447802513834063, 23.87744830687368491, -60.53680291695862081 ) ) ;
#4776 = EDGE_CURVE ( 'NONE', #5656, #13337, #18797, .T. ) ;
#4777 = AXIS2_PLACEMENT_3D ( 'NONE', #20057, #12923, #16606 ) ;
#4778 = CARTESIAN_POINT ( 'NONE',  ( -12.70473862104220153, 11.99136930790643163, 44.75655646380171504 ) ) ;
#4779 = VERTEX_POINT ( 'NONE', #7849 ) ;
#4780 = ORIENTED_EDGE ( 'NONE', *, *, #12686, .T. ) ;
#4781 = CIRCLE ( 'NONE', #7695, 5.000000000000000000 ) ;
#4782 = EDGE_LOOP ( 'NONE', ( #10278, #9271, #17612, #1740 ) ) ;
#4783 = CARTESIAN_POINT ( 'NONE',  ( -18.43720426449199223, 27.80056269872155283, 57.71457384195534956 ) ) ;
#4784 = DIRECTION ( 'NONE',  ( -0.000000000000000000, -0.000000000000000000, -1.000000000000000000 ) ) ;
#4785 = CARTESIAN_POINT ( 'NONE',  ( -14.06256854266897705, 5.693415384482571895, -58.85512087818929672 ) ) ;
#4786 = DIRECTION ( 'NONE',  ( 0.000000000000000000, 1.000000000000000000, 0.000000000000000000 ) ) ;
#4787 = AXIS2_PLACEMENT_3D ( 'NONE', #16115, #9024, #2263 ) ;
#4788 = ORIENTED_EDGE ( 'NONE', *, *, #423, .T. ) ;
#4789 = DIRECTION ( 'NONE',  ( 0.000000000000000000, 1.000000000000000000, 0.000000000000000000 ) ) ;
#4790 = CARTESIAN_POINT ( 'NONE',  ( -4.465627739065156199, 40.00000000000001421, -51.33835364202109020 ) ) ;
#4791 = CARTESIAN_POINT ( 'NONE',  ( -1.387778780781445518E-14, 20.00000000000000355, -102.9999999999999716 ) ) ;
#4792 = FACE_OUTER_BOUND ( 'NONE', #14709, .T. ) ;
#4793 = EDGE_CURVE ( 'NONE', #11430, #19192, #15111, .T. ) ;
#4794 = VERTEX_POINT ( 'NONE', #16097 ) ;
#4795 = CARTESIAN_POINT ( 'NONE',  ( 24.65063509461093361, 12.50000000000006750, -5.000000000000004441 ) ) ;
#4796 = ORIENTED_EDGE ( 'NONE', *, *, #20868, .F. ) ;
#4797 = CARTESIAN_POINT ( 'NONE',  ( 25.00000000000000000, -20.00000000000000000, -24.99999999999999289 ) ) ;
#4798 = FACE_OUTER_BOUND ( 'NONE', #17306, .T. ) ;
#4799 = FACE_BOUND ( 'NONE', #2257, .T. ) ;
#4800 = VECTOR ( 'NONE', #19302, 999.9999999999998863 ) ;
#4801 = VERTEX_POINT ( 'NONE', #634 ) ;
#4802 = AXIS2_PLACEMENT_3D ( 'NONE', #11284, #11395, #18380 ) ;
#4803 = ORIENTED_EDGE ( 'NONE', *, *, #22363, .T. ) ;
#4804 = CARTESIAN_POINT ( 'NONE',  ( -5.761861175224586518, -0.6790081076912936053, 52.02240682770946023 ) ) ;
#4805 = ADVANCED_FACE ( 'NONE', ( #19667 ), #7440, .T. ) ;
#4806 = DIRECTION ( 'NONE',  ( 6.505213034913038160E-19, 3.903127820947822896E-18, 1.000000000000000000 ) ) ;
#4807 = B_SPLINE_CURVE_WITH_KNOTS ( 'NONE', 3,
 ( #15163, #22528, #1437, #15506 ),
 .UNSPECIFIED., .F., .F.,
 ( 4, 4 ),
 ( 0.001893031756885383459, 0.003808480026563708203 ),
 .UNSPECIFIED. ) ;
#4808 = EDGE_LOOP ( 'NONE', ( #10933, #17855 ) ) ;
#4809 = CARTESIAN_POINT ( 'NONE',  ( -34.99999999999999289, 0.000000000000000000, -3.012171160963566127E-14 ) ) ;
#4810 = AXIS2_PLACEMENT_3D ( 'NONE', #10260, #18752, #8106 ) ;
#4811 = DIRECTION ( 'NONE',  ( -0.000000000000000000, 1.000000000000000000, -0.000000000000000000 ) ) ;
#4812 = CARTESIAN_POINT ( 'NONE',  ( -13.85640646055084702, 1.500000000000008216, 11.99999999999970335 ) ) ;
#4813 = ADVANCED_FACE ( 'NONE', ( #2591 ), #11098, .F. ) ;
#4814 = CARTESIAN_POINT ( 'NONE',  ( -20.00401474702687921, 19.84140115762917489, -58.14847693657501537 ) ) ;
#4815 = DIRECTION ( 'NONE',  ( -0.000000000000000000, -0.000000000000000000, -1.000000000000000000 ) ) ;
#4816 = CARTESIAN_POINT ( 'NONE',  ( -11.24990497772101605, 36.62343892044449234, 57.74518096503233267 ) ) ;
#4817 = ORIENTED_EDGE ( 'NONE', *, *, #22265, .T. ) ;
#4818 = CARTESIAN_POINT ( 'NONE',  ( -35.00000000000000000, -5.000000000000000000, 1.387778780781445676E-14 ) ) ;
#4819 = FACE_BOUND ( 'NONE', #22108, .T. ) ;
#4820 = CARTESIAN_POINT ( 'NONE',  ( -35.00000000000000000, -5.000000000000000888, -17.99999999999998934 ) ) ;
#4821 = DIRECTION ( 'NONE',  ( 0.000000000000000000, 0.000000000000000000, 1.000000000000000000 ) ) ;
#4822 = EDGE_LOOP ( 'NONE', ( #5242, #20888, #14382, #3515 ) ) ;
#4823 = DIRECTION ( 'NONE',  ( 6.505213034913038160E-19, 3.903127820947822896E-18, 1.000000000000000000 ) ) ;
#4824 = DIRECTION ( 'NONE',  ( 6.505213034913038160E-19, 3.903127820947822896E-18, 1.000000000000000000 ) ) ;
#4825 = DIRECTION ( 'NONE',  ( -1.000000000000000000, 0.000000000000000000, 0.000000000000000000 ) ) ;
#4826 = CARTESIAN_POINT ( 'NONE',  ( 35.00000000000058265, 28.00000000000000000, -52.50000000000076739 ) ) ;
#4827 = VECTOR ( 'NONE', #17904, 1000.000000000000000 ) ;
#4828 = ORIENTED_EDGE ( 'NONE', *, *, #1766, .F. ) ;
#4829 = EDGE_CURVE ( 'NONE', #11055, #19583, #22454, .T. ) ;
#4830 = EDGE_LOOP ( 'NONE', ( #1185, #5337, #82, #725 ) ) ;
#4831 = ORIENTED_EDGE ( 'NONE', *, *, #10006, .T. ) ;
#4832 = DIRECTION ( 'NONE',  ( -6.505213034913038160E-19, -3.903127820947822896E-18, -1.000000000000000000 ) ) ;
#4833 = CARTESIAN_POINT ( 'NONE',  ( 7.980461308160213818, -36.39375341857525825, -2.999999999999999112 ) ) ;
#4834 = CYLINDRICAL_SURFACE ( 'NONE', #1105, 2.500000000000002220 ) ;
#4835 = CARTESIAN_POINT ( 'NONE',  ( -25.00000000000000000, 20.00000000000000000, 6.487780019669002523E-15 ) ) ;
#4836 = DIRECTION ( 'NONE',  ( 1.000000000000000000, 0.000000000000000000, 0.000000000000000000 ) ) ;
#4837 = VERTEX_POINT ( 'NONE', #2242 ) ;
#4838 = LINE ( 'NONE', #8722, #12759 ) ;
#4839 = DIRECTION ( 'NONE',  ( 0.000000000000000000, 0.000000000000000000, -1.000000000000000000 ) ) ;
#4840 = ORIENTED_EDGE ( 'NONE', *, *, #9555, .F. ) ;
#4841 = ADVANCED_FACE ( 'NONE', ( #12651 ), #7514, .F. ) ;
#4842 = EDGE_CURVE ( 'NONE', #9799, #10690, #2971, .T. ) ;
#4843 = LINE ( 'NONE', #11813, #4300 ) ;
#4844 = DIRECTION ( 'NONE',  ( 0.000000000000000000, 0.000000000000000000, 1.000000000000000000 ) ) ;
#4845 = AXIS2_PLACEMENT_3D ( 'NONE', #5739, #17767, #352 ) ;
#4846 = CARTESIAN_POINT ( 'NONE',  ( -35.00000000000000000, -15.00000000000000000, -14.99999999999997691 ) ) ;
#4847 = CYLINDRICAL_SURFACE ( 'NONE', #3137, 19.11328065563151313 ) ;
#4848 = ORIENTED_EDGE ( 'NONE', *, *, #8479, .T. ) ;
#4849 = DIRECTION ( 'NONE',  ( -6.505213034913038160E-19, -3.903127820947822896E-18, -1.000000000000000000 ) ) ;
#4850 = ORIENTED_EDGE ( 'NONE', *, *, #18415, .T. ) ;
#4851 = CARTESIAN_POINT ( 'NONE',  ( -35.00000000000058265, 26.00000000000000355, -55.00000000000076028 ) ) ;
#4852 = CARTESIAN_POINT ( 'NONE',  ( -14.34650594848455896, 37.25275621493270251, 56.33443587181654522 ) ) ;
#4853 = ORIENTED_EDGE ( 'NONE', *, *, #12898, .F. ) ;
#4854 = PLANE ( 'NONE',  #10166 ) ;
#4855 = DIRECTION ( 'NONE',  ( -0.000000000000000000, -1.000000000000000000, -0.000000000000000000 ) ) ;
#4856 = DIRECTION ( 'NONE',  ( -6.505213034913038160E-19, -3.903127820947822896E-18, -1.000000000000000000 ) ) ;
#4857 = CARTESIAN_POINT ( 'NONE',  ( 16.64903669412982978, 31.11586081922178337, -59.71532480898645900 ) ) ;
#4858 = ORIENTED_EDGE ( 'NONE', *, *, #6484, .T. ) ;
#4859 = AXIS2_PLACEMENT_3D ( 'NONE', #7419, #14275, #17961 ) ;
#4860 = VERTEX_POINT ( 'NONE', #16555 ) ;
#4861 = ADVANCED_FACE ( 'NONE', ( #20005 ), #17823, .T. ) ;
#4862 = ORIENTED_EDGE ( 'NONE', *, *, #15313, .F. ) ;
#4863 = CARTESIAN_POINT ( 'NONE',  ( 35.00000000000000000, 7.000000000000000000, 41.00000000000002132 ) ) ;
#4864 = VECTOR ( 'NONE', #16190, 1000.000000000000000 ) ;
#4865 = ORIENTED_EDGE ( 'NONE', *, *, #9290, .F. ) ;
#4866 = CARTESIAN_POINT ( 'NONE',  ( 35.00000000000000000, 17.00000000000000000, 2.365113165210053967E-14 ) ) ;
#4867 = LINE ( 'NONE', #13888, #5896 ) ;
#4868 = ORIENTED_EDGE ( 'NONE', *, *, #17392, .T. ) ;
#4869 = CARTESIAN_POINT ( 'NONE',  ( -35.00000000000000000, 22.00000000000000355, 2.365113165210053967E-14 ) ) ;
#4870 = CARTESIAN_POINT ( 'NONE',  ( -9.327259721472405118, -2.742977016014211511, -53.40697688051520942 ) ) ;
#4871 = ORIENTED_EDGE ( 'NONE', *, *, #22619, .F. ) ;
#4872 = CARTESIAN_POINT ( 'NONE',  ( -2.670518050928090137, 14.42800760928497539, 8.613211112165400252 ) ) ;
#4873 = ORIENTED_EDGE ( 'NONE', *, *, #171, .F. ) ;
#4874 = CARTESIAN_POINT ( 'NONE',  ( 7.073833244813752863, 38.72384638770318332, -54.13588498570150165 ) ) ;
#4875 = CARTESIAN_POINT ( 'NONE',  ( 4.080045426412937104, -32.20238537491820807, 2.999999999999995559 ) ) ;
#4876 = CARTESIAN_POINT ( 'NONE',  ( -34.99999999999999289, -5.000000000000000000, 59.99999999999698019 ) ) ;
#4877 = CARTESIAN_POINT ( 'NONE',  ( -18.85684496195311866, 26.68267098057082976, -60.33873919100125960 ) ) ;
#4878 = EDGE_CURVE ( 'NONE', #18308, #22383, #7725, .T. ) ;
#4879 = AXIS2_PLACEMENT_3D ( 'NONE', #17880, #9167, #7447 ) ;
#4880 = EDGE_CURVE ( 'NONE', #21115, #17014, #16910, .T. ) ;
#4881 = AXIS2_PLACEMENT_3D ( 'NONE', #18988, #17593, #22542 ) ;
#4882 = CARTESIAN_POINT ( 'NONE',  ( 9.689843208404422370, 39.33333333333334281, -54.54983754392748097 ) ) ;
#4883 = EDGE_CURVE ( 'NONE', #14834, #22210, #22173, .T. ) ;
#4884 = ORIENTED_EDGE ( 'NONE', *, *, #18355, .F. ) ;
#4885 = ORIENTED_EDGE ( 'NONE', *, *, #9185, .T. ) ;
#4886 = ORIENTED_EDGE ( 'NONE', *, *, #908, .T. ) ;
#4887 = ORIENTED_EDGE ( 'NONE', *, *, #11836, .F. ) ;
#4888 = FACE_OUTER_BOUND ( 'NONE', #21108, .T. ) ;
#4889 = CARTESIAN_POINT ( 'NONE',  ( -6.000000000000000888, 0.000000000000000000, -5.999999999999998224 ) ) ;
#4890 = AXIS2_PLACEMENT_3D ( 'NONE', #2626, #21874, #11324 ) ;
#4891 = CIRCLE ( 'NONE', #21004, 16.99999999999998579 ) ;
#4892 = CARTESIAN_POINT ( 'NONE',  ( 2.247165119384746834, 39.96957922271067787, -50.40104177638675509 ) ) ;
#4893 = FACE_OUTER_BOUND ( 'NONE', #14989, .T. ) ;
#4894 = DIRECTION ( 'NONE',  ( -0.000000000000000000, -1.000000000000000000, -0.000000000000000000 ) ) ;
#4895 = VECTOR ( 'NONE', #13052, 1000.000000000000000 ) ;
#4896 = ORIENTED_EDGE ( 'NONE', *, *, #1987, .F. ) ;
#4897 = CYLINDRICAL_SURFACE ( 'NONE', #12016, 2.500000000000002220 ) ;
#4898 = CARTESIAN_POINT ( 'NONE',  ( -2.026529067239271509, 40.00000000000000711, -49.98891171552928370 ) ) ;
#4899 = DIRECTION ( 'NONE',  ( -1.000000000000000000, -9.002681209562842834E-16, 0.000000000000000000 ) ) ;
#4900 = CARTESIAN_POINT ( 'NONE',  ( 10.43027093729823562, 39.22757009021513142, -54.80615623442508877 ) ) ;
#4901 = AXIS2_PLACEMENT_3D ( 'NONE', #765, #647, #7748 ) ;
#4902 = ORIENTED_EDGE ( 'NONE', *, *, #21257, .F. ) ;
#4903 = CARTESIAN_POINT ( 'NONE',  ( 28.95348479018586119, -14.76298474240533842, 3.000000000000023537 ) ) ;
#4904 = ORIENTED_EDGE ( 'NONE', *, *, #18911, .F. ) ;
#4905 = AXIS2_PLACEMENT_3D ( 'NONE', #10050, #13370, #4697 ) ;
#4906 = DIRECTION ( 'NONE',  ( 0.000000000000000000, 0.000000000000000000, -1.000000000000000000 ) ) ;
#4907 = CARTESIAN_POINT ( 'NONE',  ( 5.999999999999999112, 0.000000000000000000, -6.000000000000000000 ) ) ;
#4908 = CARTESIAN_POINT ( 'NONE',  ( 34.99999999999980105, 24.73819270004212356, 54.99999999999922551 ) ) ;
#4909 = AXIS2_PLACEMENT_3D ( 'NONE', #19921, #11086, #2515 ) ;
#4910 = EDGE_LOOP ( 'NONE', ( #21437, #15265, #15159, #5765 ) ) ;
#4911 = ADVANCED_FACE ( 'NONE', ( #18732 ), #16496, .F. ) ;
#4912 = ORIENTED_EDGE ( 'NONE', *, *, #19091, .F. ) ;
#4913 = CARTESIAN_POINT ( 'NONE',  ( -3.021476695451119188, -1.097455775060080407, 50.32853965771198546 ) ) ;
#4914 = VECTOR ( 'NONE', #6786, 1000.000000000000000 ) ;
#4915 = DIRECTION ( 'NONE',  ( 6.505213034913038160E-19, 3.903127820947822896E-18, 1.000000000000000000 ) ) ;
#4916 = ORIENTED_EDGE ( 'NONE', *, *, #4129, .T. ) ;
#4917 = EDGE_CURVE ( 'NONE', #5723, #4700, #5895, .T. ) ;
#4918 = CARTESIAN_POINT ( 'NONE',  ( 9.852267639826642665, 8.683574217357131531, 43.21671877549180607 ) ) ;
#4919 = AXIS2_PLACEMENT_3D ( 'NONE', #18298, #20477, #9820 ) ;
#4920 = CARTESIAN_POINT ( 'NONE',  ( -5.999999999999999112, -40.00000000000000000, 6.000000000000001776 ) ) ;
#4921 = DIRECTION ( 'NONE',  ( -1.000000000000000000, 0.000000000000000000, 3.063596499322170048E-16 ) ) ;
#4922 = CARTESIAN_POINT ( 'NONE',  ( -22.29034605647555978, 17.39518641927480047, -58.63862881473036026 ) ) ;
#4923 = AXIS2_PLACEMENT_3D ( 'NONE', #8814, #2046, #7426 ) ;
#4924 = CARTESIAN_POINT ( 'NONE',  ( -11.38359864655678777, 29.79463497853557996, -44.07478837098127400 ) ) ;
#4925 = CARTESIAN_POINT ( 'NONE',  ( -9.829668860677969633, 37.49547983895929804, 57.11616152306119432 ) ) ;
#4926 = ORIENTED_EDGE ( 'NONE', *, *, #4032, .F. ) ;
#4927 = CARTESIAN_POINT ( 'NONE',  ( 6.426802710256914963, 33.56875711009141838, 41.03786381671501005 ) ) ;
#4928 = CARTESIAN_POINT ( 'NONE',  ( 11.05758567243059609, 3.294696707144193493, -55.18338768060583277 ) ) ;
#4929 = DIRECTION ( 'NONE',  ( 0.000000000000000000, -1.000000000000000000, 0.000000000000000000 ) ) ;
#4930 = ORIENTED_EDGE ( 'NONE', *, *, #12380, .T. ) ;
#4931 = CIRCLE ( 'NONE', #19946, 1.999999999999999778 ) ;
#4932 = CARTESIAN_POINT ( 'NONE',  ( -24.99999999999999645, 20.00000000000000000, 16.50000000000000355 ) ) ;
#4933 = DIRECTION ( 'NONE',  ( 8.659560562354892183E-17, 0.7071067811865507924, -0.7071067811865441310 ) ) ;
#4934 = DIRECTION ( 'NONE',  ( -0.000000000000000000, 1.000000000000000000, -0.000000000000000000 ) ) ;
#4935 = CIRCLE ( 'NONE', #2746, 2.500000000000002220 ) ;
#4936 = EDGE_CURVE ( 'NONE', #20460, #19594, #18693, .T. ) ;
#4937 = ORIENTED_EDGE ( 'NONE', *, *, #1020, .F. ) ;
#4938 = PRODUCT_CONTEXT ( 'NONE', #20143, 'mechanical' ) ;
#4939 = AXIS2_PLACEMENT_3D ( 'NONE', #13473, #896, #1010 ) ;
#4940 = ORIENTED_EDGE ( 'NONE', *, *, #15419, .F. ) ;
#4941 = CARTESIAN_POINT ( 'NONE',  ( 15.00428685838202725, -32.89708536800409178, 2.932460736555828618 ) ) ;
#4942 = CARTESIAN_POINT ( 'NONE',  ( -0.003185071962412873176, 13.00000169078104051, 8.999999436406458386 ) ) ;
#4943 = CARTESIAN_POINT ( 'NONE',  ( -13.85640646055073333, -1.500000000000011768, -8.000000000000493827 ) ) ;
#4944 = CARTESIAN_POINT ( 'NONE',  ( 3.608224830031758756E-13, -2.775557561562891351E-14, -4.999999999999997335 ) ) ;
#4945 = CIRCLE ( 'NONE', #3066, 19.11328065563151313 ) ;
#4946 = DIRECTION ( 'NONE',  ( -0.000000000000000000, -1.000000000000000000, -0.000000000000000000 ) ) ;
#4947 = EDGE_LOOP ( 'NONE', ( #21975, #2184, #13909, #4047, #7264 ) ) ;
#4948 = DIRECTION ( 'NONE',  ( 0.000000000000000000, 0.5150380749100562650, 0.8571673007021111124 ) ) ;
#4949 = DIRECTION ( 'NONE',  ( 0.000000000000000000, 1.000000000000000000, 0.000000000000000000 ) ) ;
#4950 = VERTEX_POINT ( 'NONE', #2702 ) ;
#4951 = CARTESIAN_POINT ( 'NONE',  ( 34.99999999999980815, 40.00000000000000000, 54.99999999999922551 ) ) ;
#4952 = CARTESIAN_POINT ( 'NONE',  ( -2.999999999999999112, 16.00000000000000000, 8.485281374238567764 ) ) ;
#4953 = CIRCLE ( 'NONE', #17383, 2.000000000000001776 ) ;
#4954 = CARTESIAN_POINT ( 'NONE',  ( 24.65063509461118230, 12.50000000000006750, -2.999999999999988898 ) ) ;
#4955 = EDGE_LOOP ( 'NONE', ( #12141, #20649, #6787, #14295 ) ) ;
#4956 = CARTESIAN_POINT ( 'NONE',  ( 14.92530643917651823, 21.54450079162174347, -45.79309713780074986 ) ) ;
#4957 = ORIENTED_EDGE ( 'NONE', *, *, #19973, .T. ) ;
#4958 = CARTESIAN_POINT ( 'NONE',  ( 25.00000000000000000, 20.00000000000000000, 6.487780019669002523E-15 ) ) ;
#4959 = CARTESIAN_POINT ( 'NONE',  ( -20.89512770937652775, 28.22558907592242150, 58.31975796628790931 ) ) ;
#4960 = ORIENTED_EDGE ( 'NONE', *, *, #6883, .T. ) ;
#4961 = CARTESIAN_POINT ( 'NONE',  ( -35.00000000000000000, 0.000000000000000000, 2.365113165210053967E-14 ) ) ;
#4962 = EDGE_CURVE ( 'NONE', #4023, #18629, #514, .T. ) ;
#4963 = DIRECTION ( 'NONE',  ( 0.000000000000000000, -1.000000000000000000, 0.000000000000000000 ) ) ;
#4964 = DIRECTION ( 'NONE',  ( 1.296372316667914327E-16, 1.000000000000000000, -0.000000000000000000 ) ) ;
#4965 = CIRCLE ( 'NONE', #17753, 36.76383501243555685 ) ;
#4966 = CIRCLE ( 'NONE', #19955, 60.00000000000000000 ) ;
#4967 = CARTESIAN_POINT ( 'NONE',  ( 13.03660953228075492, 4.807999378483715169, -58.46122805341365591 ) ) ;
#4968 = CIRCLE ( 'NONE', #8984, 19.11328065563152023 ) ;
#4969 = EDGE_CURVE ( 'NONE', #21483, #14094, #22406, .T. ) ;
#4970 = EDGE_LOOP ( 'NONE', ( #16703, #7390, #4111, #15223 ) ) ;
#4971 = VERTEX_POINT ( 'NONE', #15155 ) ;
#4972 = VERTEX_POINT ( 'NONE', #7972 ) ;
#4973 = CARTESIAN_POINT ( 'NONE',  ( 48.93401015228424455, 10.00000000000000000, -46.57614213197967956 ) ) ;
#4974 = ORIENTED_EDGE ( 'NONE', *, *, #17616, .F. ) ;
#4975 = CARTESIAN_POINT ( 'NONE',  ( 35.00000000000001421, 0.000000000000000000, 39.00000000000002132 ) ) ;
#4976 = CARTESIAN_POINT ( 'NONE',  ( 17.21639554191072818, 34.43961005730907488, 57.30688911148507714 ) ) ;
#4977 = CARTESIAN_POINT ( 'NONE',  ( 9.727694841165407169, 39.99999999999998579, -53.57919902740184881 ) ) ;
#4978 = ADVANCED_FACE ( 'NONE', ( #15387 ), #12063, .T. ) ;
#4979 = ORIENTED_EDGE ( 'NONE', *, *, #9058, .T. ) ;
#4980 = CARTESIAN_POINT ( 'NONE',  ( -25.00000000000000000, -20.00000000000000000, 6.487780019669002523E-15 ) ) ;
#4981 = CARTESIAN_POINT ( 'NONE',  ( 89.99999999999701572, 0.000000000000000000, 2.499999999999956479 ) ) ;
#4982 = ORIENTED_EDGE ( 'NONE', *, *, #4221, .F. ) ;
#4983 = CIRCLE ( 'NONE', #6815, 16.49999999999999645 ) ;
#4984 = FACE_OUTER_BOUND ( 'NONE', #990, .T. ) ;
#4985 = AXIS2_PLACEMENT_3D ( 'NONE', #3643, #17601, #1907 ) ;
#4986 = CONICAL_SURFACE ( 'NONE', #2409, 2.524999999999999467, 0.7853981633973095011 ) ;
#4987 = ADVANCED_BREP_SHAPE_REPRESENTATION ( '', ( #10654, #18273 ), #22681 ) ;
#4988 = ORIENTED_EDGE ( 'NONE', *, *, #19505, .T. ) ;
#4989 = DIRECTION ( 'NONE',  ( -0.000000000000000000, 1.000000000000000000, -0.000000000000000000 ) ) ;
#4990 = EDGE_CURVE ( 'NONE', #15385, #548, #10897, .T. ) ;
#4991 = DIRECTION ( 'NONE',  ( -6.505213034913038160E-19, -3.903127820947822896E-18, -1.000000000000000000 ) ) ;
#4992 = CARTESIAN_POINT ( 'NONE',  ( 42.50000000000000711, -5.000000000000000000, 54.00000000000000711 ) ) ;
#4993 = FACE_OUTER_BOUND ( 'NONE', #20761, .T. ) ;
#4994 = ADVANCED_FACE ( 'NONE', ( #1540 ), #15729, .T. ) ;
#4995 = DIRECTION ( 'NONE',  ( 0.000000000000000000, -0.000000000000000000, -1.000000000000000000 ) ) ;
#4996 = CARTESIAN_POINT ( 'NONE',  ( -15.00000000000001421, 19.61444766276327556, 45.82575694955841072 ) ) ;
#4997 = CIRCLE ( 'NONE', #19634, 19.11328065563151668 ) ;
#4998 = VECTOR ( 'NONE', #14731, 1000.000000000000000 ) ;
#4999 = EDGE_CURVE ( 'NONE', #12985, #6209, #9557, .T. ) ;
#5000 = AXIS2_PLACEMENT_3D ( 'NONE', #3127, #11609, #15369 ) ;
#5001 = ORIENTED_EDGE ( 'NONE', *, *, #17328, .F. ) ;
#5002 = AXIS2_PLACEMENT_3D ( 'NONE', #5712, #9259, #9387 ) ;
#5003 = VERTEX_POINT ( 'NONE', #13988 ) ;
#5004 = VERTEX_POINT ( 'NONE', #4981 ) ;
#5005 = EDGE_CURVE ( 'NONE', #57, #13636, #3270, .T. ) ;
#5006 = ORIENTED_EDGE ( 'NONE', *, *, #6978, .F. ) ;
#5007 = DIRECTION ( 'NONE',  ( -0.000000000000000000, -1.000000000000000000, -0.000000000000000000 ) ) ;
#5008 = CIRCLE ( 'NONE', #22582, 1.000000000000000888 ) ;
#5009 = DIRECTION ( 'NONE',  ( -1.000000000000000000, 0.000000000000000000, 0.000000000000000000 ) ) ;
#5010 = FACE_OUTER_BOUND ( 'NONE', #17802, .T. ) ;
#5011 = DIRECTION ( 'NONE',  ( 0.000000000000000000, 0.000000000000000000, -1.000000000000000000 ) ) ;
#5012 = EDGE_CURVE ( 'NONE', #8634, #22398, #15947, .T. ) ;
#5013 = ORIENTED_EDGE ( 'NONE', *, *, #2072, .F. ) ;
#5014 = CARTESIAN_POINT ( 'NONE',  ( 0.000000000000000000, -1.500000000000015099, 0.000000000000000000 ) ) ;
#5015 = CARTESIAN_POINT ( 'NONE',  ( -4.719078656571195296, 39.99999999999999289, -51.46810812756150000 ) ) ;
#5016 = FACE_OUTER_BOUND ( 'NONE', #21485, .T. ) ;
#5017 = LINE ( 'NONE', #19103, #2776 ) ;
#5018 = AXIS2_PLACEMENT_3D ( 'NONE', #8916, #3557, #1832 ) ;
#5019 = DIRECTION ( 'NONE',  ( -0.000000000000000000, -0.000000000000000000, -1.000000000000000000 ) ) ;
#5020 = EDGE_LOOP ( 'NONE', ( #15013, #11391 ) ) ;
#5021 = CARTESIAN_POINT ( 'NONE',  ( -22.98755168577423902, -22.97438720605751783, -6.999999999999950262 ) ) ;
#5022 = CARTESIAN_POINT ( 'NONE',  ( 32.35999952201609631, -1.423424233832876196, -6.999999999999999112 ) ) ;
#5023 = VECTOR ( 'NONE', #20204, 1000.000000000000000 ) ;
#5024 = VERTEX_POINT ( 'NONE', #10570 ) ;
#5025 = DIRECTION ( 'NONE',  ( -6.505213034913038160E-19, -3.903127820947822896E-18, -1.000000000000000000 ) ) ;
#5026 = CARTESIAN_POINT ( 'NONE',  ( 32.10132595304146719, 5.074925817841635656, -2.999999999999971578 ) ) ;
#5027 = DIRECTION ( 'NONE',  ( -1.000000000000000000, 2.141938622189920653E-14, 0.000000000000000000 ) ) ;
#5028 = ORIENTED_EDGE ( 'NONE', *, *, #16309, .T. ) ;
#5029 = AXIS2_PLACEMENT_3D ( 'NONE', #379, #9319, #7372 ) ;
#5030 = CONICAL_SURFACE ( 'NONE', #18186, 2.524999999999999467, 0.7853981633973095011 ) ;
#5031 = ADVANCED_FACE ( 'NONE', ( #259, #5210, #8860 ), #20793, .F. ) ;
#5032 = ORIENTED_EDGE ( 'NONE', *, *, #777, .T. ) ;
#5033 = CARTESIAN_POINT ( 'NONE',  ( -8.526039741978737041, -2.856534014484948258, 52.89583463521491780 ) ) ;
#5034 = LINE ( 'NONE', #6406, #18207 ) ;
#5035 = ORIENTED_EDGE ( 'NONE', *, *, #4401, .F. ) ;
#5036 = CARTESIAN_POINT ( 'NONE',  ( 11.38359864655677711, 10.20536502146444313, 44.07478837098129532 ) ) ;
#5037 =( BOUNDED_SURFACE ( )  B_SPLINE_SURFACE ( 3, 2, ( 
 ( #18850, #20568, #18736 ),
 ( #8196, #1545, #22525 ),
 ( #3157, #22648, #6821 ),
 ( #13784, #8645, #20800 ),
 ( #20916, #4874, #5112 ),
 ( #11741, #15620, #13442 ),
 ( #19079, #3386, #11630 ),
 ( #9911, #18633, #2938 ),
 ( #1315, #8308, #7379 ),
 ( #385, #10920, #10676 ),
 ( #21352, #15737, #12191 ),
 ( #21134, #14459, #7489 ),
 ( #3619, #17682, #3501 ),
 ( #19310, #5217, #9102 ) ),
 .UNSPECIFIED., .F., .F., .F. ) 
 B_SPLINE_SURFACE_WITH_KNOTS ( ( 4, 2, 2, 2, 2, 2, 4 ),
 ( 3, 3 ),
 ( 0.004259382447192485224, 0.005809352080732410606, 0.007359321714272335120, 0.008909291347812259634, 0.01045926098135218502, 0.01355920024843203578, 0.01665913951551188654 ),
 ( 0.1636502049369185086, 1.000000000000000000 ),
 .UNSPECIFIED. ) 
 GEOMETRIC_REPRESENTATION_ITEM ( )  RATIONAL_B_SPLINE_SURFACE ( (
 ( 0.9022234441951376693, 0.7012635705450175339, 1.000000000000000000),
 ( 0.9123774980386742950, 0.7322872220199752036, 1.000000000000000000),
 ( 0.9211831106396635160, 0.7591909848486969592, 1.000000000000000000),
 ( 0.9369226144573956638, 0.8072798455494799574, 1.000000000000000000),
 ( 0.9438532932728125324, 0.8284551285810179966, 1.000000000000000000),
 ( 0.9562652441348715726, 0.8663773263162527494, 1.000000000000000000),
 ( 0.9617542084831443017, 0.8831477432869754285, 1.000000000000000000),
 ( 0.9714480778053882215, 0.9127653943188843710, 1.000000000000000000),
 ( 0.9756417576472291575, 0.9255783322661890189, 1.000000000000000000),
 ( 0.9865757101953547270, 0.9589848060079729786, 1.000000000000000000),
 ( 0.9916868072432731829, 0.9746007261037917813, 1.000000000000000000),
 ( 0.9984050148984049411, 0.9951268466110081423, 1.000000000000000000),
 ( 0.9999940431410754282, 0.9999818000260773943, 1.000000000000000000),
 ( 1.000000000000000000, 1.000000000000000000, 1.000000000000000000) ) ) 
 REPRESENTATION_ITEM ( '' )  SURFACE ( )  );
#5038 = CIRCLE ( 'NONE', #14531, 10.00000000000000000 ) ;
#5039 = EDGE_CURVE ( 'NONE', #3941, #8689, #18560, .T. ) ;
#5040 = AXIS2_PLACEMENT_3D ( 'NONE', #16164, #4613, #16633 ) ;
#5041 = CARTESIAN_POINT ( 'NONE',  ( -0.5279010140432128795, 35.00028092684671321, -38.73355033370099676 ) ) ;
#5042 = DIRECTION ( 'NONE',  ( 0.000000000000000000, 0.000000000000000000, -1.000000000000000000 ) ) ;
#5043 = CARTESIAN_POINT ( 'NONE',  ( -16.71858216490109328, 8.984148545335303382, -57.18548413420069210 ) ) ;
#5044 = FACE_OUTER_BOUND ( 'NONE', #12991, .T. ) ;
#5045 = CIRCLE ( 'NONE', #6872, 0.9999999999999974465 ) ;
#5046 = ORIENTED_EDGE ( 'NONE', *, *, #10998, .T. ) ;
#5047 = DIRECTION ( 'NONE',  ( -6.505213034913038160E-19, -3.903127820947822896E-18, -1.000000000000000000 ) ) ;
#5048 = AXIS2_PLACEMENT_3D ( 'NONE', #3914, #17764, #21209 ) ;
#5049 = FILL_AREA_STYLE_COLOUR ( '', #2721 ) ;
#5050 = FACE_BOUND ( 'NONE', #7550, .T. ) ;
#5051 = CARTESIAN_POINT ( 'NONE',  ( 7.197698565811989191, 35.43359966464129229, 2.932460736555801972 ) ) ;
#5052 = AXIS2_PLACEMENT_3D ( 'NONE', #18777, #13485, #9946 ) ;
#5053 = VERTEX_POINT ( 'NONE', #5428 ) ;
#5054 = CYLINDRICAL_SURFACE ( 'NONE', #6065, 0.9999999999999974465 ) ;
#5055 = CARTESIAN_POINT ( 'NONE',  ( -35.00000000000058265, 40.00000000000000711, -55.00000000000076028 ) ) ;
#5056 = CARTESIAN_POINT ( 'NONE',  ( -34.99999999999999289, 5.000000000000000000, 9.000000000000007105 ) ) ;
#5057 = EDGE_CURVE ( 'NONE', #4131, #3734, #6491, .T. ) ;
#5058 = AXIS2_PLACEMENT_3D ( 'NONE', #10271, #15535, #22561 ) ;
#5059 = ORIENTED_EDGE ( 'NONE', *, *, #17176, .T. ) ;
#5060 = CIRCLE ( 'NONE', #22275, 2.500000000000002220 ) ;
#5061 = AXIS2_PLACEMENT_3D ( 'NONE', #20760, #15802, #17196 ) ;
#5062 = AXIS2_PLACEMENT_3D ( 'NONE', #15392, #5113, #20681 ) ;
#5063 = SHAPE_DEFINITION_REPRESENTATION ( #14396, #3430 ) ;
#5064 = VECTOR ( 'NONE', #13684, 1000.000000000000000 ) ;
#5065 = ORIENTED_EDGE ( 'NONE', *, *, #20954, .F. ) ;
#5066 = CARTESIAN_POINT ( 'NONE',  ( 13.00000000000024336, -2.516660498395250745, 60.00099999999999767 ) ) ;
#5067 = CARTESIAN_POINT ( 'NONE',  ( -1.572625745558603239, 13.32985487263095159, 8.879522542765043269 ) ) ;
#5068 = DIRECTION ( 'NONE',  ( 0.000000000000000000, -1.000000000000000000, 0.000000000000000000 ) ) ;
#5069 = LINE ( 'NONE', #19267, #15993 ) ;
#5070 = DIRECTION ( 'NONE',  ( 6.505213034913038160E-19, 3.903127820947822896E-18, 1.000000000000000000 ) ) ;
#5071 = VERTEX_POINT ( 'NONE', #11961 ) ;
#5072 = DIRECTION ( 'NONE',  ( -1.000000000000000000, 0.000000000000000000, 0.000000000000000000 ) ) ;
#5073 = CARTESIAN_POINT ( 'NONE',  ( -11.89435616776549232, 40.00000000000000000, -54.28884887643229007 ) ) ;
#5074 = ORIENTED_EDGE ( 'NONE', *, *, #20274, .F. ) ;
#5075 = DIRECTION ( 'NONE',  ( 6.505213034913038160E-19, 3.903127820947822896E-18, 1.000000000000000000 ) ) ;
#5076 = CARTESIAN_POINT ( 'NONE',  ( 1.734786545154649763E-13, -25.00000000000000000, -16.00000000000029488 ) ) ;
#5077 = CARTESIAN_POINT ( 'NONE',  ( 22.22891329980564024, -23.65408649739134006, -2.999999999999971578 ) ) ;
#5078 = CARTESIAN_POINT ( 'NONE',  ( 3.801357092295314821, 39.91216781786773282, 51.45795407606280492 ) ) ;
#5079 = CARTESIAN_POINT ( 'NONE',  ( 14.87996495114178153, 21.93329436794036269, -45.77322900830822761 ) ) ;
#5080 = AXIS2_PLACEMENT_3D ( 'NONE', #5853, #576, #21431 ) ;
#5081 = ORIENTED_EDGE ( 'NONE', *, *, #14388, .F. ) ;
#5082 = DIRECTION ( 'NONE',  ( -6.505213034913038160E-19, -3.903127820947822896E-18, -1.000000000000000000 ) ) ;
#5083 = CARTESIAN_POINT ( 'NONE',  ( -21.07599011712229853, 12.09199673218657622, 58.36745205258139890 ) ) ;
#5084 = EDGE_CURVE ( 'NONE', #20516, #11968, #22519, .T. ) ;
#5085 = AXIS2_PLACEMENT_3D ( 'NONE', #21491, #2132, #11287 ) ;
#5086 = ORIENTED_EDGE ( 'NONE', *, *, #15228, .T. ) ;
#5087 = LINE ( 'NONE', #17096, #12345 ) ;
#5088 = AXIS2_PLACEMENT_3D ( 'NONE', #21868, #6167, #3723 ) ;
#5089 = CARTESIAN_POINT ( 'NONE',  ( -25.00000000000000000, 20.00000000000000000, 6.487780019669002523E-15 ) ) ;
#5090 = CARTESIAN_POINT ( 'NONE',  ( 23.74488952252801255, -25.58633464742643326, -2.999999999999978240 ) ) ;
#5091 = ADVANCED_FACE ( 'NONE', ( #3381 ), #16741, .F. ) ;
#5092 = B_SPLINE_SURFACE_WITH_KNOTS ( 'NONE', 1, 3, ( 
 ( #12049, #3351, #114, #7107, #12376, #19386 ),
 ( #17305, #1395, #11928, #1622, #8603, #453 ) ),
 .UNSPECIFIED., .F., .F., .F.,
 ( 2, 2 ),
 ( 4, 2, 4 ),
 ( 0.000000000000000000, 1.000000000000000000 ),
 ( 0.000000000000000000, 0.001214050925806517758, 0.002428101851613035517 ),
 .UNSPECIFIED. ) ;
#5093 = PLANE ( 'NONE',  #12578 ) ;
#5094 = B_SPLINE_CURVE_WITH_KNOTS ( 'NONE', 3,
 ( #14929, #21954, #6246, #2930, #13202, #9903, #16892, #8185, #15149, #22169, #6469, #13431, #13546, #18840, #3265, #36, #12292, #10564, #3374, #15382, #8410, #5101 ),
 .UNSPECIFIED., .F., .F.,
 ( 4, 2, 2, 2, 2, 2, 2, 2, 2, 2, 4 ),
 ( 0.000000000000000000, 0.1250000000000004163, 0.2500000000000008327, 0.3750000000000012212, 0.4375000000000012212, 0.5000000000000012212, 0.6250000000000012212, 0.7500000000000011102, 0.8750000000000011102, 0.9375000000000005551, 1.000000000000000000 ),
 .UNSPECIFIED. ) ;
#5095 = ORIENTED_EDGE ( 'NONE', *, *, #1897, .T. ) ;
#5096 = ORIENTED_EDGE ( 'NONE', *, *, #12555, .F. ) ;
#5097 = B_SPLINE_CURVE_WITH_KNOTS ( 'NONE', 3,
 ( #4615, #15011, #18810, #22027, #11595, #17077, #18589, #16865, #15354, #22373, #6660, #2898, #9874, #8156, #13618, #18923 ),
 .UNSPECIFIED., .F., .F.,
 ( 4, 2, 2, 2, 2, 2, 2, 4 ),
 ( 0.000000000000000000, 0.004782611835060866790, 0.005978264793826080885, 0.007173917752591294113, 0.009565223670121721436, 0.01195652958765214442, 0.01434783550518256914, 0.01913044734024342899 ),
 .UNSPECIFIED. ) ;
#5098 = ORIENTED_EDGE ( 'NONE', *, *, #775, .T. ) ;
#5099 = FACE_OUTER_BOUND ( 'NONE', #1982, .T. ) ;
#5100 = EDGE_LOOP ( 'NONE', ( #9016, #2700, #3271, #1805 ) ) ;
#5101 = CARTESIAN_POINT ( 'NONE',  ( -2.999999999999998668, 22.00000000000000355, 6.485281374238567764 ) ) ;
#5102 = CARTESIAN_POINT ( 'NONE',  ( 20.16756852208514772, 29.88972976525005976, 58.13897502025236719 ) ) ;
#5103 = CARTESIAN_POINT ( 'NONE',  ( -13.00000000000011546, 42.51666049839536043, -105.0010000000000048 ) ) ;
#5104 = EDGE_CURVE ( 'NONE', #21718, #19773, #20400, .T. ) ;
#5105 = ORIENTED_EDGE ( 'NONE', *, *, #10161, .T. ) ;
#5106 = DIRECTION ( 'NONE',  ( -1.000000000000000000, 1.301042606982605814E-16, 0.000000000000000000 ) ) ;
#5107 = CARTESIAN_POINT ( 'NONE',  ( -18.00000000000001421, 20.00000000000000711, 102.0000000000000142 ) ) ;
#5108 = ORIENTED_EDGE ( 'NONE', *, *, #1839, .F. ) ;
#5109 =( GEOMETRIC_REPRESENTATION_CONTEXT ( 3 ) GLOBAL_UNCERTAINTY_ASSIGNED_CONTEXT ( ( #22046 ) ) GLOBAL_UNIT_ASSIGNED_CONTEXT ( ( #17664, #12495, #475 ) ) REPRESENTATION_CONTEXT ( 'NONE', 'WORKASPACE' ) );
#5110 = FACE_OUTER_BOUND ( 'NONE', #2891, .T. ) ;
#5111 = ORIENTED_EDGE ( 'NONE', *, *, #4022, .T. ) ;
#5112 = CARTESIAN_POINT ( 'NONE',  ( 6.433485051968857782, 38.94088993357618733, -55.16018527339313238 ) ) ;
#5113 = DIRECTION ( 'NONE',  ( 6.505213034913038160E-19, 3.903127820947822896E-18, 1.000000000000000000 ) ) ;
#5114 = EDGE_CURVE ( 'NONE', #21949, #3635, #5764, .T. ) ;
#5115 = DIRECTION ( 'NONE',  ( -1.000000000000000000, -1.208970125616060101E-17, 6.505213034913038160E-19 ) ) ;
#5116 = DIRECTION ( 'NONE',  ( -1.000000000000000000, -1.208970125616060717E-17, 0.000000000000000000 ) ) ;
#5117 = AXIS2_PLACEMENT_3D ( 'NONE', #4456, #6051, #11432 ) ;
#5118 = CARTESIAN_POINT ( 'NONE',  ( 2.775557561562891351E-14, -2.775557561562891351E-14, 2.999999999999999112 ) ) ;
#5119 = CARTESIAN_POINT ( 'NONE',  ( 3.330669073875469621E-13, -1.110223024625156540E-13, -2.999999999999971578 ) ) ;
#5120 = CARTESIAN_POINT ( 'NONE',  ( -0.8626474017859412369, -36.14481870267513131, 2.932969818539080453 ) ) ;
#5121 = ORIENTED_EDGE ( 'NONE', *, *, #6388, .F. ) ;
#5122 = VERTEX_POINT ( 'NONE', #14572 ) ;
#5123 = ORIENTED_EDGE ( 'NONE', *, *, #9302, .F. ) ;
#5124 = VERTEX_POINT ( 'NONE', #19970 ) ;
#5125 = CARTESIAN_POINT ( 'NONE',  ( 13.00000000000024336, -2.516660498395250745, -105.0000000000000142 ) ) ;
#5126 = EDGE_CURVE ( 'NONE', #11767, #20985, #19755, .T. ) ;
#5127 = AXIS2_PLACEMENT_3D ( 'NONE', #7091, #19132, #14171 ) ;
#5128 = DIRECTION ( 'NONE',  ( -3.063596499322170048E-16, -0.000000000000000000, -1.000000000000000000 ) ) ;
#5129 = DIRECTION ( 'NONE',  ( 0.000000000000000000, 0.000000000000000000, 1.000000000000000000 ) ) ;
#5130 = CARTESIAN_POINT ( 'NONE',  ( 6.675595648756416089, 39.71118687073258258, 53.17234506582082787 ) ) ;
#5131 = ORIENTED_EDGE ( 'NONE', *, *, #13212, .F. ) ;
#5132 = FACE_OUTER_BOUND ( 'NONE', #12353, .T. ) ;
#5133 = CARTESIAN_POINT ( 'NONE',  ( -2.274190298599449100, 40.00000000000000000, -50.13372678551965578 ) ) ;
#5134 = ADVANCED_FACE ( 'NONE', ( #2097 ), #18133, .T. ) ;
#5135 = DIRECTION ( 'NONE',  ( 1.000000000000000000, 1.208970125616053321E-17, 0.000000000000000000 ) ) ;
#5136 = ADVANCED_FACE ( 'NONE', ( #829 ), #12962, .F. ) ;
#5137 = CARTESIAN_POINT ( 'NONE',  ( -34.90673715956756240, 2.733356359154242119E-14, 5.750000000000001776 ) ) ;
#5138 = DIRECTION ( 'NONE',  ( -6.505213034913038160E-19, -3.903127820947822896E-18, -1.000000000000000000 ) ) ;
#5139 = EDGE_CURVE ( 'NONE', #18701, #11842, #13593, .T. ) ;
#5140 = CIRCLE ( 'NONE', #19411, 2.500000000000002220 ) ;
#5141 = VERTEX_POINT ( 'NONE', #4060 ) ;
#5142 = CARTESIAN_POINT ( 'NONE',  ( -11.93830856187180700, -33.47097213929440329, 3.000000000000063061 ) ) ;
#5143 = CARTESIAN_POINT ( 'NONE',  ( -15.58771758597476875, 32.56665981830160916, 59.37826087086043714 ) ) ;
#5144 = ORIENTED_EDGE ( 'NONE', *, *, #15319, .T. ) ;
#5145 = DIRECTION ( 'NONE',  ( 0.000000000000000000, 0.000000000000000000, -1.000000000000000000 ) ) ;
#5146 = VECTOR ( 'NONE', #15309, 1000.000000000000000 ) ;
#5147 = DIRECTION ( 'NONE',  ( -0.000000000000000000, -0.000000000000000000, -1.000000000000000000 ) ) ;
#5148 = DIRECTION ( 'NONE',  ( 0.000000000000000000, 0.000000000000000000, -1.000000000000000000 ) ) ;
#5149 = ORIENTED_EDGE ( 'NONE', *, *, #3561, .F. ) ;
#5150 = ORIENTED_EDGE ( 'NONE', *, *, #11126, .T. ) ;
#5151 = ORIENTED_EDGE ( 'NONE', *, *, #303, .F. ) ;
#5152 = DIRECTION ( 'NONE',  ( -6.505213034913038160E-19, -3.903127820947822896E-18, -1.000000000000000000 ) ) ;
#5153 = VECTOR ( 'NONE', #16231, 1000.000000000000114 ) ;
#5154 = CARTESIAN_POINT ( 'NONE',  ( 35.00000000000000000, 17.00000000000000000, -38.99999999999999289 ) ) ;
#5155 = ORIENTED_EDGE ( 'NONE', *, *, #20962, .F. ) ;
#5156 = FACE_OUTER_BOUND ( 'NONE', #9966, .T. ) ;
#5157 = CARTESIAN_POINT ( 'NONE',  ( -5.422195817667174289, 33.99281763503099540, -40.31637036980814770 ) ) ;
#5158 = FACE_OUTER_BOUND ( 'NONE', #5317, .T. ) ;
#5159 = CARTESIAN_POINT ( 'NONE',  ( -19.02718446893024762, 26.17927818496970716, -57.88297158504751394 ) ) ;
#5160 = PLANE ( 'NONE',  #16283 ) ;
#5161 = VERTEX_POINT ( 'NONE', #12847 ) ;
#5162 = DIRECTION ( 'NONE',  ( 1.000000000000000000, 0.000000000000000000, -1.445602896647339163E-16 ) ) ;
#5163 = CARTESIAN_POINT ( 'NONE',  ( -1.387778780781445518E-14, 20.00000000000000355, -105.0000000000000142 ) ) ;
#5164 = LINE ( 'NONE', #19135, #5610 ) ;
#5165 = EDGE_CURVE ( 'NONE', #6470, #8079, #16069, .T. ) ;
#5166 = ORIENTED_EDGE ( 'NONE', *, *, #5233, .T. ) ;
#5167 = EDGE_CURVE ( 'NONE', #8307, #5279, #5045, .T. ) ;
#5168 = CARTESIAN_POINT ( 'NONE',  ( 25.99999999999998579, 19.99999999999999645, -105.0000000000000142 ) ) ;
#5169 = CARTESIAN_POINT ( 'NONE',  ( 7.943521403985130338E-15, 0.000000000000000000, -47.49736834814795827 ) ) ;
#5170 = ADVANCED_FACE ( 'NONE', ( #5882 ), #14336, .F. ) ;
#5171 = ORIENTED_EDGE ( 'NONE', *, *, #17634, .T. ) ;
#5172 = APPLICATION_PROTOCOL_DEFINITION ( 'draft international standard', 'automotive_design', 1998, #18977 ) ;
#5173 = ORIENTED_EDGE ( 'NONE', *, *, #4764, .F. ) ;
#5174 = CARTESIAN_POINT ( 'NONE',  ( 15.12081897056688540, -33.51030287062373247, 2.800654218530485018 ) ) ;
#5175 = DIRECTION ( 'NONE',  ( -0.000000000000000000, 1.000000000000000000, -0.000000000000000000 ) ) ;
#5176 = DIRECTION ( 'NONE',  ( 0.000000000000000000, 0.000000000000000000, -1.000000000000000000 ) ) ;
#5177 = CARTESIAN_POINT ( 'NONE',  ( -35.00000000000058975, 24.73819270004212356, -55.00000000000076028 ) ) ;
#5178 = CARTESIAN_POINT ( 'NONE',  ( 89.99999999999701572, 0.000000000000000000, -5.216535399428728743E-14 ) ) ;
#5179 = ORIENTED_EDGE ( 'NONE', *, *, #10704, .F. ) ;
#5180 = DIRECTION ( 'NONE',  ( -6.505213034913038160E-19, -3.903127820947822896E-18, -1.000000000000000000 ) ) ;
#5181 = CARTESIAN_POINT ( 'NONE',  ( -7.524443153164861897, 20.67323765728989926, -5.000000000000004441 ) ) ;
#5182 = ORIENTED_EDGE ( 'NONE', *, *, #303, .T. ) ;
#5183 = CARTESIAN_POINT ( 'NONE',  ( 10.27431133777637484, -4.928932188134504955, -51.43682631505696179 ) ) ;
#5184 = CARTESIAN_POINT ( 'NONE',  ( 20.34735785252014395, 29.47800210776922469, -58.18363580933384327 ) ) ;
#5185 = DIRECTION ( 'NONE',  ( 0.000000000000000000, 0.5150380749100562650, 0.8571673007021111124 ) ) ;
#5186 = CARTESIAN_POINT ( 'NONE',  ( 8.118562860349435084, 39.55762401320047417, 53.90122740908830679 ) ) ;
#5187 = CARTESIAN_POINT ( 'NONE',  ( 2.220446049250313081E-13, 2.775557561562891351E-14, -2.800654218530485018 ) ) ;
#5188 = ORIENTED_EDGE ( 'NONE', *, *, #4077, .F. ) ;
#5189 = CARTESIAN_POINT ( 'NONE',  ( -42.50000000000000711, -12.00000000000000000, 47.50000000000000711 ) ) ;
#5190 = DIRECTION ( 'NONE',  ( 0.000000000000000000, 1.000000000000000000, 0.000000000000000000 ) ) ;
#5191 = ORIENTED_EDGE ( 'NONE', *, *, #10332, .T. ) ;
#5192 = CYLINDRICAL_SURFACE ( 'NONE', #648, 19.11328065563150957 ) ;
#5193 = VECTOR ( 'NONE', #2440, 1000.000000000000000 ) ;
#5194 = CIRCLE ( 'NONE', #2253, 19.11328065563150957 ) ;
#5195 = DIRECTION ( 'NONE',  ( 1.000000000000000000, 0.000000000000000000, 0.000000000000000000 ) ) ;
#5196 = DIRECTION ( 'NONE',  ( -0.000000000000000000, 1.000000000000000000, -0.000000000000000000 ) ) ;
#5197 = PLANE ( 'NONE',  #7478 ) ;
#5198 = ORIENTED_EDGE ( 'NONE', *, *, #10974, .T. ) ;
#5199 = ORIENTED_EDGE ( 'NONE', *, *, #15001, .F. ) ;
#5200 = VERTEX_POINT ( 'NONE', #4164 ) ;
#5201 = DIRECTION ( 'NONE',  ( -1.000000000000000000, 1.264902534566421922E-16, 0.000000000000000000 ) ) ;
#5202 = ADVANCED_FACE ( 'NONE', ( #7594 ), #18013, .F. ) ;
#5203 = ORIENTED_EDGE ( 'NONE', *, *, #16776, .F. ) ;
#5204 = CARTESIAN_POINT ( 'NONE',  ( 17.96165932904279572, 6.521477064918314248, 57.53061250216241973 ) ) ;
#5205 = CIRCLE ( 'NONE', #1912, 36.76383501243555685 ) ;
#5206 = CARTESIAN_POINT ( 'NONE',  ( 6.910515180469714913, 40.00000000000002132, -52.51112560306592059 ) ) ;
#5207 = CARTESIAN_POINT ( 'NONE',  ( 3.397749794379752331, 40.00000000000000000, 50.77335383852931727 ) ) ;
#5208 = ORIENTED_EDGE ( 'NONE', *, *, #11829, .T. ) ;
#5209 = LINE ( 'NONE', #1539, #5790 ) ;
#5210 = FACE_BOUND ( 'NONE', #2225, .T. ) ;
#5211 = ORIENTED_EDGE ( 'NONE', *, *, #794, .F. ) ;
#5212 = CARTESIAN_POINT ( 'NONE',  ( 35.00000000000058265, 40.00000000000000000, -55.00000000000076028 ) ) ;
#5213 = EDGE_CURVE ( 'NONE', #16803, #13092, #2479, .T. ) ;
#5214 = ORIENTED_EDGE ( 'NONE', *, *, #14943, .F. ) ;
#5215 = CARTESIAN_POINT ( 'NONE',  ( 7.776554266669417956E-15, -4.648749848372173865, -45.43309249825056639 ) ) ;
#5216 = ORIENTED_EDGE ( 'NONE', *, *, #10356, .T. ) ;
#5217 = CARTESIAN_POINT ( 'NONE',  ( -2.782727930551067045E-14, 40.00000000000000000, -48.73397172404478539 ) ) ;
#5218 = CARTESIAN_POINT ( 'NONE',  ( -35.00000000000000000, 40.00000000000000000, 1.387778780781445676E-14 ) ) ;
#5219 = CARTESIAN_POINT ( 'NONE',  ( -0.7618512339543030976, 39.99660974252569901, 49.31784456962214591 ) ) ;
#5220 = DIRECTION ( 'NONE',  ( -6.505213034913038160E-19, -3.903127820947822896E-18, -1.000000000000000000 ) ) ;
#5221 = CARTESIAN_POINT ( 'NONE',  ( -13.06969024216325970, -19.15111107797470780, -4.999999999999969802 ) ) ;
#5222 = DIRECTION ( 'NONE',  ( -1.000000000000000000, -1.208970125616060717E-17, 0.000000000000000000 ) ) ;
#5223 = ADVANCED_FACE ( 'NONE', ( #727 ), #5529, .T. ) ;
#5224 = VERTEX_POINT ( 'NONE', #3825 ) ;
#5225 = EDGE_LOOP ( 'NONE', ( #419, #21595, #15652, #18243 ) ) ;
#5226 = ORIENTED_EDGE ( 'NONE', *, *, #7212, .F. ) ;
#5227 = EDGE_CURVE ( 'NONE', #260, #19833, #19683, .T. ) ;
#5228 = EDGE_LOOP ( 'NONE', ( #12581, #8173, #21367, #17267 ) ) ;
#5229 = DIRECTION ( 'NONE',  ( 0.000000000000000000, 0.000000000000000000, -1.000000000000000000 ) ) ;
#5230 = DIRECTION ( 'NONE',  ( -1.000000000000000000, 0.000000000000000000, 0.000000000000000000 ) ) ;
#5231 = CARTESIAN_POINT ( 'NONE',  ( -30.60042966911705165, -7.474202570536076173, 3.000000000000023537 ) ) ;
#5232 = CARTESIAN_POINT ( 'NONE',  ( 0.09252246807544707574, 39.99995033533620870, 48.80586619582643237 ) ) ;
#5233 = EDGE_CURVE ( 'NONE', #15126, #668, #21690, .T. ) ;
#5234 = AXIS2_PLACEMENT_3D ( 'NONE', #18219, #9734, #14760 ) ;
#5235 = ORIENTED_EDGE ( 'NONE', *, *, #17003, .F. ) ;
#5236 = CARTESIAN_POINT ( 'NONE',  ( 12.00937115242647835, 34.74700806321096280, 2.800654218530512551 ) ) ;
#5237 = DIRECTION ( 'NONE',  ( 0.000000000000000000, 0.000000000000000000, 1.000000000000000000 ) ) ;
#5238 = DIRECTION ( 'NONE',  ( 1.296372316667914327E-16, 1.000000000000000000, -0.000000000000000000 ) ) ;
#5239 = CARTESIAN_POINT ( 'NONE',  ( -35.00000000000000000, 17.00000000000000000, 2.365113165210053967E-14 ) ) ;
#5240 = SURFACE_SIDE_STYLE ('',( #20708 ) ) ;
#5241 = AXIS2_PLACEMENT_3D ( 'NONE', #22282, #4856, #11826 ) ;
#5242 = ORIENTED_EDGE ( 'NONE', *, *, #15883, .F. ) ;
#5243 = CARTESIAN_POINT ( 'NONE',  ( -27.64365646977265456, -17.09029715894952517, -2.999999999999981792 ) ) ;
#5244 = CARTESIAN_POINT ( 'NONE',  ( 1.387778780781445676E-14, -5.000000000000000000, -48.73397172404115452 ) ) ;
#5245 = ADVANCED_FACE ( 'NONE', ( #2214 ), #9196, .T. ) ;
#5246 = DIRECTION ( 'NONE',  ( 0.000000000000000000, -1.000000000000000000, 0.000000000000000000 ) ) ;
#5247 = FACE_BOUND ( 'NONE', #17588, .T. ) ;
#5248 = B_SPLINE_CURVE_WITH_KNOTS ( 'NONE', 3,
 ( #10425, #12159, #9065, #19606, #5507, #12479, #234, #17647, #351, #14309, #3915, #10643, #8607, #17424, #7009, #10540, #19491, #7228, #3798, #15585, #17765, #6904, #16041, #5616, #13866, #13965, #20882, #5184, #1743, #8726, #8833, #15703, #18, #20989, #5294, #17544, #118, #11223, #16386, #7683 ),
 .UNSPECIFIED., .F., .F.,
 ( 4, 2, 2, 2, 2, 2, 2, 2, 2, 2, 2, 2, 2, 2, 2, 2, 2, 2, 2, 4 ),
 ( 0.000000000000000000, 0.002766773850155581499, 0.004150160775233378320, 0.005533547700311174274, 0.008300321550466765314, 0.009683708475544557798, 0.01106709540062235028, 0.01660064310093351328, 0.01798403002601130229, 0.01936741695108909131, 0.02213419080124466587, 0.02490096465140024390, 0.02766773850155581846, 0.03043451235171139649, 0.03181789927678917856, 0.03320128620186695717, 0.03873483390217812017, 0.04011822082725590571, 0.04150160775233369126, 0.04426838160248925541 ),
 .UNSPECIFIED. ) ;
#5249 = ORIENTED_EDGE ( 'NONE', *, *, #18573, .F. ) ;
#5250 = ORIENTED_EDGE ( 'NONE', *, *, #431, .F. ) ;
#5251 = CIRCLE ( 'NONE', #3837, 25.00000000000000000 ) ;
#5252 = EDGE_CURVE ( 'NONE', #2560, #20709, #14450, .T. ) ;
#5253 = ADVANCED_FACE ( 'NONE', ( #16869 ), #11369, .T. ) ;
#5254 = AXIS2_PLACEMENT_3D ( 'NONE', #12489, #19616, #17896 ) ;
#5255 = VERTEX_POINT ( 'NONE', #11708 ) ;
#5256 = CARTESIAN_POINT ( 'NONE',  ( 2.419767991124955664, -3.149022461041079968, -49.02154318835233227 ) ) ;
#5257 = DIRECTION ( 'NONE',  ( 0.000000000000000000, 0.000000000000000000, 1.000000000000000000 ) ) ;
#5258 = ORIENTED_EDGE ( 'NONE', *, *, #20161, .T. ) ;
#5259 = CARTESIAN_POINT ( 'NONE',  ( -28.50000000000001421, 19.99999999999982947, 105.0000000000000142 ) ) ;
#5260 = CARTESIAN_POINT ( 'NONE',  ( -7.711478842616581453, 31.57187188083529605, -7.000000000000006217 ) ) ;
#5261 = CARTESIAN_POINT ( 'NONE',  ( -29.14949368109861894, 11.93972437435542133, 2.999999999999995559 ) ) ;
#5262 = CARTESIAN_POINT ( 'NONE',  ( -17.35828117057637954, 30.07901706856257817, -57.39628071425624256 ) ) ;
#5263 = DIRECTION ( 'NONE',  ( 0.000000000000000000, 0.000000000000000000, -1.000000000000000000 ) ) ;
#5264 = B_SPLINE_SURFACE_WITH_KNOTS ( 'NONE', 1, 3, ( 
 ( #21434, #9620, #4038, #579, #11453, #18102, #12823, #19836, #11114, #806, #12932, #2418, #9407, #19942, #14766, #6077, #4369, #11346, #16613, #7913 ),
 ( #14873, #21899, #6195, #13159, #22234, #1250, #13598, #11898, #13491, #20736, #6300, #18903, #2757, #17058, #8468, #9953, #15437, #8243, #3090, #6754 ) ),
 .UNSPECIFIED., .F., .F., .F.,
 ( 2, 2 ),
 ( 4, 2, 2, 2, 2, 2, 2, 2, 2, 4 ),
 ( 0.000000000000000000, 1.000000000000000000 ),
 ( -4.246609446761914828E-05, 0.0006546318687081847335, 0.001351729831883988642, 0.002048827795059792768, 0.002745925758235596460, 0.004140121684587204712, 0.005534317610938812096, 0.006928513537290420347, 0.008322709463642028599, 0.01111110131634524337 ),
 .UNSPECIFIED. ) ;
#5265 = AXIS2_PLACEMENT_3D ( 'NONE', #2512, #11200, #16704 ) ;
#5266 = VERTEX_POINT ( 'NONE', #6105 ) ;
#5267 = LINE ( 'NONE', #9033, #14509 ) ;
#5268 = SURFACE_SIDE_STYLE ('',( #20512 ) ) ;
#5269 = CIRCLE ( 'NONE', #22105, 49.99999999999998579 ) ;
#5270 = EDGE_CURVE ( 'NONE', #21037, #21090, #2146, .T. ) ;
#5271 = FACE_OUTER_BOUND ( 'NONE', #8780, .T. ) ;
#5272 = LINE ( 'NONE', #11789, #21724 ) ;
#5273 = AXIS2_PLACEMENT_3D ( 'NONE', #11909, #19141, #4825 ) ;
#5274 = ORIENTED_EDGE ( 'NONE', *, *, #364, .F. ) ;
#5275 = EDGE_CURVE ( 'NONE', #11150, #10311, #18947, .T. ) ;
#5276 = PLANE ( 'NONE',  #1316 ) ;
#5277 = CARTESIAN_POINT ( 'NONE',  ( -35.00000000000058265, 28.00000000000000000, -55.00000000000076028 ) ) ;
#5278 = AXIS2_PLACEMENT_3D ( 'NONE', #14122, #6946, #5222 ) ;
#5279 = VERTEX_POINT ( 'NONE', #3116 ) ;
#5280 = AXIS2_PLACEMENT_3D ( 'NONE', #17506, #8803, #17384 ) ;
#5281 = AXIS2_PLACEMENT_3D ( 'NONE', #7089, #3216, #15441 ) ;
#5282 = ADVANCED_FACE ( 'NONE', ( #9649 ), #15259, .T. ) ;
#5283 = ORIENTED_EDGE ( 'NONE', *, *, #10191, .T. ) ;
#5284 = CARTESIAN_POINT ( 'NONE',  ( 21.41958700883258970, 27.56232195404059837, 3.000000000000002665 ) ) ;
#5285 = CARTESIAN_POINT ( 'NONE',  ( -1.039655021832126547, -3.147609295952968456, 46.52691668518833268 ) ) ;
#5286 = CARTESIAN_POINT ( 'NONE',  ( -31.21605069118058040, -8.646032897229122938, -6.999999999999999112 ) ) ;
#5287 = CARTESIAN_POINT ( 'NONE',  ( -10.99584631063772378, 3.272668205460793178, 57.61971594758626480 ) ) ;
#5288 = DIRECTION ( 'NONE',  ( 6.505213034913038160E-19, 3.903127820947822896E-18, 1.000000000000000000 ) ) ;
#5289 = VERTEX_POINT ( 'NONE', #16640 ) ;
#5290 = DIRECTION ( 'NONE',  ( 0.000000000000000000, 0.000000000000000000, -1.000000000000000000 ) ) ;
#5291 = DIRECTION ( 'NONE',  ( -1.000000000000000000, -3.103995799953189701E-14, 0.000000000000000000 ) ) ;
#5292 = VERTEX_POINT ( 'NONE', #7940 ) ;
#5293 = CARTESIAN_POINT ( 'NONE',  ( 2.220446049250313081E-13, 2.775557561562891351E-14, -2.800654218530485018 ) ) ;
#5294 = CARTESIAN_POINT ( 'NONE',  ( 15.34956869069047869, 36.37910824616916017, -56.69201590313573291 ) ) ;
#5295 = DIRECTION ( 'NONE',  ( -0.4166911066143236253, 0.000000000000000000, 0.9090481404571104651 ) ) ;
#5296 = CARTESIAN_POINT ( 'NONE',  ( 22.97438720605771323, -22.98755168577421060, -7.000000000000006217 ) ) ;
#5297 = CARTESIAN_POINT ( 'NONE',  ( 7.017626609043924546, 33.27455722914837821, -41.44244536674933244 ) ) ;
#5298 = ORIENTED_EDGE ( 'NONE', *, *, #13947, .F. ) ;
#5299 = DIRECTION ( 'NONE',  ( 0.000000000000000000, 1.000000000000000000, 0.000000000000000000 ) ) ;
#5300 = VECTOR ( 'NONE', #5962, 1000.000000000000000 ) ;
#5301 = CARTESIAN_POINT ( 'NONE',  ( -21.63981290377905253, 13.82170478134237612, 58.49475859713705006 ) ) ;
#5302 = VECTOR ( 'NONE', #18204, 1000.000000000000000 ) ;
#5303 = VERTEX_POINT ( 'NONE', #20537 ) ;
#5304 = CARTESIAN_POINT ( 'NONE',  ( 12.10743492717617364, 1.299801688893591267, 55.43551573822927026 ) ) ;
#5305 = CARTESIAN_POINT ( 'NONE',  ( -34.99999999999999289, -3.999999999999985345, -3.012171160963566127E-14 ) ) ;
#5306 = FACE_OUTER_BOUND ( 'NONE', #5955, .T. ) ;
#5307 = ORIENTED_EDGE ( 'NONE', *, *, #11043, .F. ) ;
#5308 = ORIENTED_EDGE ( 'NONE', *, *, #14749, .T. ) ;
#5309 = ORIENTED_EDGE ( 'NONE', *, *, #12414, .F. ) ;
#5310 = ADVANCED_FACE ( 'NONE', ( #18469 ), #21927, .T. ) ;
#5311 = ORIENTED_EDGE ( 'NONE', *, *, #12688, .F. ) ;
#5312 = DIRECTION ( 'NONE',  ( -1.000000000000000000, -0.000000000000000000, -0.000000000000000000 ) ) ;
#5313 = AXIS2_PLACEMENT_3D ( 'NONE', #15586, #2385, #7113 ) ;
#5314 = CARTESIAN_POINT ( 'NONE',  ( 20.89754528720908411, 28.21939688025627291, 58.32034131438403790 ) ) ;
#5315 = DIRECTION ( 'NONE',  ( 0.000000000000000000, 0.000000000000000000, 1.000000000000000000 ) ) ;
#5316 = CYLINDRICAL_SURFACE ( 'NONE', #5847, 0.9999999999999974465 ) ;
#5317 = EDGE_LOOP ( 'NONE', ( #10062, #14422, #7754, #15956 ) ) ;
#5318 = CARTESIAN_POINT ( 'NONE',  ( -35.00000000000000000, 10.00000000000000000, 2.365113165210053967E-14 ) ) ;
#5319 = EDGE_LOOP ( 'NONE', ( #12095, #20816, #15192, #3114 ) ) ;
#5320 = CARTESIAN_POINT ( 'NONE',  ( -7.505578006075204200, 1.461761173328241847, 55.63523492904089096 ) ) ;
#5321 = CARTESIAN_POINT ( 'NONE',  ( 35.43359966464143440, -7.197698565811765370, 2.932460736555821512 ) ) ;
#5322 = ORIENTED_EDGE ( 'NONE', *, *, #10596, .T. ) ;
#5323 = CARTESIAN_POINT ( 'NONE',  ( -35.00000000000000000, 7.000000000000000000, 2.365113165210053967E-14 ) ) ;
#5324 = EDGE_CURVE ( 'NONE', #16900, #943, #9053, .T. ) ;
#5325 = ORIENTED_EDGE ( 'NONE', *, *, #17045, .F. ) ;
#5326 = LINE ( 'NONE', #17805, #3514 ) ;
#5327 = AXIS2_PLACEMENT_3D ( 'NONE', #19082, #13903, #6393 ) ;
#5328 = CARTESIAN_POINT ( 'NONE',  ( -6.696867368503558448E-15, 40.00000000000000000, -48.73397172404479960 ) ) ;
#5329 = DIRECTION ( 'NONE',  ( 1.000000000000000000, -0.000000000000000000, -0.000000000000000000 ) ) ;
#5330 = CARTESIAN_POINT ( 'NONE',  ( 17.18568680885866584, 30.37812028685803156, 59.88587632367774205 ) ) ;
#5331 = CARTESIAN_POINT ( 'NONE',  ( 2.602085213965210642E-15, 5.025303850726727362, 0.000000000000000000 ) ) ;
#5332 = EDGE_CURVE ( 'NONE', #8764, #10311, #11483, .T. ) ;
#5333 = AXIS2_PLACEMENT_3D ( 'NONE', #8447, #6501, #3304 ) ;
#5334 = CARTESIAN_POINT ( 'NONE',  ( 15.50000000000024336, -2.516660498395250745, -105.0010000000000048 ) ) ;
#5335 = ORIENTED_EDGE ( 'NONE', *, *, #12367, .T. ) ;
#5336 = ADVANCED_FACE ( 'NONE', ( #20314 ), #18814, .T. ) ;
#5337 = ORIENTED_EDGE ( 'NONE', *, *, #20910, .F. ) ;
#5338 = EDGE_LOOP ( 'NONE', ( #21977, #8939 ) ) ;
#5339 = AXIS2_PLACEMENT_3D ( 'NONE', #13110, #863, #13214 ) ;
#5340 = VERTEX_POINT ( 'NONE', #20429 ) ;
#5341 = FACE_OUTER_BOUND ( 'NONE', #14223, .T. ) ;
#5342 = CARTESIAN_POINT ( 'NONE',  ( -11.98990878915331848, -34.11307262910443683, -2.932164912090521547 ) ) ;
#5343 = VECTOR ( 'NONE', #18510, 1000.000000000000000 ) ;
#5344 = DIRECTION ( 'NONE',  ( 0.000000000000000000, 0.000000000000000000, -1.000000000000000000 ) ) ;
#5345 = DIRECTION ( 'NONE',  ( 1.000000000000000000, 0.000000000000000000, 0.000000000000000000 ) ) ;
#5346 = AXIS2_PLACEMENT_3D ( 'NONE', #5168, #3676, #14059 ) ;
#5347 = CARTESIAN_POINT ( 'NONE',  ( 1.943361993987648306, 39.97741573862661824, 50.18563611142815972 ) ) ;
#5348 = VECTOR ( 'NONE', #10037, 1000.000000000000000 ) ;
#5349 = ORIENTED_EDGE ( 'NONE', *, *, #10128, .T. ) ;
#5350 = DIRECTION ( 'NONE',  ( 6.505213034913038160E-19, 3.903127820947822896E-18, 1.000000000000000000 ) ) ;
#5351 = DIRECTION ( 'NONE',  ( 1.000000000000000000, 0.000000000000000000, 0.000000000000000000 ) ) ;
#5352 = DIRECTION ( 'NONE',  ( -1.000000000000000000, 1.296372316667914327E-16, 0.000000000000000000 ) ) ;
#5353 = CYLINDRICAL_SURFACE ( 'NONE', #19254, 18.00000000000000000 ) ;
#5354 = DIRECTION ( 'NONE',  ( 0.000000000000000000, -1.000000000000000000, 0.000000000000000000 ) ) ;
#5355 = AXIS2_PLACEMENT_3D ( 'NONE', #19864, #16297, #18136 ) ;
#5356 = VECTOR ( 'NONE', #5378, 1000.000000000000000 ) ;
#5357 = CARTESIAN_POINT ( 'NONE',  ( -9.375631618502383802, 39.53999972426225185, 54.37753810704350599 ) ) ;
#5358 = CARTESIAN_POINT ( 'NONE',  ( -34.99999999999980815, 26.00000000000000355, 54.99999999999922551 ) ) ;
#5359 = DIRECTION ( 'NONE',  ( 0.000000000000000000, 0.000000000000000000, -1.000000000000000000 ) ) ;
#5360 = VERTEX_POINT ( 'NONE', #15015 ) ;
#5361 = EDGE_CURVE ( 'NONE', #19717, #22344, #7818, .T. ) ;
#5362 = VECTOR ( 'NONE', #13243, 1000.000000000000000 ) ;
#5363 = ORIENTED_EDGE ( 'NONE', *, *, #22321, .F. ) ;
#5364 = ORIENTED_EDGE ( 'NONE', *, *, #21013, .F. ) ;
#5365 = DIRECTION ( 'NONE',  ( 6.505213034913038160E-19, 3.903127820947822896E-18, 1.000000000000000000 ) ) ;
#5366 = DIRECTION ( 'NONE',  ( -1.000000000000000000, -1.208970125616044077E-17, 0.000000000000000000 ) ) ;
#5367 = AXIS2_PLACEMENT_3D ( 'NONE', #15335, #6641, #17520 ) ;
#5368 = FACE_OUTER_BOUND ( 'NONE', #19665, .T. ) ;
#5369 = EDGE_CURVE ( 'NONE', #11978, #1700, #1279, .T. ) ;
#5370 = FACE_OUTER_BOUND ( 'NONE', #10000, .T. ) ;
#5371 = CARTESIAN_POINT ( 'NONE',  ( -25.00000000000000000, 20.00000000000000000, 6.487780019669002523E-15 ) ) ;
#5372 = LINE ( 'NONE', #3666, #8701 ) ;
#5373 = FACE_OUTER_BOUND ( 'NONE', #5880, .T. ) ;
#5374 = AXIS2_PLACEMENT_3D ( 'NONE', #14380, #3540, #12550 ) ;
#5375 = VERTEX_POINT ( 'NONE', #4393 ) ;
#5376 = CARTESIAN_POINT ( 'NONE',  ( 7.094908322883425100, -35.33352588067112521, -6.999999999999950262 ) ) ;
#5377 = DIRECTION ( 'NONE',  ( 1.296372316667914327E-16, 1.000000000000000000, -0.000000000000000000 ) ) ;
#5378 = DIRECTION ( 'NONE',  ( 6.505213034913038160E-19, 3.903127820947822896E-18, 1.000000000000000000 ) ) ;
#5379 = EDGE_CURVE ( 'NONE', #13337, #21700, #1167, .T. ) ;
#5380 = EDGE_CURVE ( 'NONE', #11353, #21378, #3569, .T. ) ;
#5381 = CARTESIAN_POINT ( 'NONE',  ( 14.68506606271058956, 16.91806408329021494, -45.68712064066588141 ) ) ;
#5382 = ORIENTED_EDGE ( 'NONE', *, *, #1066, .F. ) ;
#5383 = CARTESIAN_POINT ( 'NONE',  ( 34.99999999999980815, 39.97500000000000142, 57.49999999999921840 ) ) ;
#5384 = CIRCLE ( 'NONE', #18183, 36.76383501243555685 ) ;
#5385 = DIRECTION ( 'NONE',  ( 0.000000000000000000, 0.000000000000000000, -1.000000000000000000 ) ) ;
#5386 = VERTEX_POINT ( 'NONE', #6442 ) ;
#5387 = ORIENTED_EDGE ( 'NONE', *, *, #22535, .F. ) ;
#5388 = DIRECTION ( 'NONE',  ( 0.000000000000000000, 0.000000000000000000, -1.000000000000000000 ) ) ;
#5389 = AXIS2_PLACEMENT_3D ( 'NONE', #11598, #6325, #10087 ) ;
#5390 = CYLINDRICAL_SURFACE ( 'NONE', #13149, 4.000000000000000000 ) ;
#5391 = FACE_OUTER_BOUND ( 'NONE', #16847, .T. ) ;
#5392 = EDGE_CURVE ( 'NONE', #18704, #13273, #18202, .T. ) ;
#5393 = CARTESIAN_POINT ( 'NONE',  ( 35.00000000000001421, -5.000000000000000000, 1.540743955509788682E-30 ) ) ;
#5394 = CONICAL_SURFACE ( 'NONE', #20045, 10.00000000000000000, 0.7853981633974447263 ) ;
#5395 = ORIENTED_EDGE ( 'NONE', *, *, #7223, .F. ) ;
#5396 = FACE_OUTER_BOUND ( 'NONE', #2996, .T. ) ;
#5397 = CARTESIAN_POINT ( 'NONE',  ( -26.65040777864139443, -24.43568323314263324, 2.932460736555830838 ) ) ;
#5398 = ORIENTED_EDGE ( 'NONE', *, *, #6147, .F. ) ;
#5399 = CARTESIAN_POINT ( 'NONE',  ( 90.00000000000000000, 40.00000000000000000, -9.108981535246192915E-16 ) ) ;
#5400 = LINE ( 'NONE', #1853, #10060 ) ;
#5401 = CARTESIAN_POINT ( 'NONE',  ( -22.00000000000001421, 20.00000000000000355, 98.00000000000000000 ) ) ;
#5402 = CARTESIAN_POINT ( 'NONE',  ( -9.952189117650787509, 40.00000000000000000, -53.64426396172093092 ) ) ;
#5403 = ORIENTED_EDGE ( 'NONE', *, *, #10283, .T. ) ;
#5404 = LINE ( 'NONE', #17429, #15206 ) ;
#5405 = EDGE_CURVE ( 'NONE', #15800, #19371, #2112, .T. ) ;
#5406 = PLANE ( 'NONE',  #13322 ) ;
#5407 = EDGE_CURVE ( 'NONE', #22593, #15748, #21137, .T. ) ;
#5408 = VERTEX_POINT ( 'NONE', #6901 ) ;
#5409 = AXIS2_PLACEMENT_3D ( 'NONE', #15480, #1636, #6914 ) ;
#5410 = AXIS2_PLACEMENT_3D ( 'NONE', #10783, #5636, #1979 ) ;
#5411 = CYLINDRICAL_SURFACE ( 'NONE', #20693, 19.11328065563150957 ) ;
#5412 = DIRECTION ( 'NONE',  ( -0.000000000000000000, -1.000000000000000000, -0.000000000000000000 ) ) ;
#5413 = VECTOR ( 'NONE', #915, 1000.000000000000000 ) ;
#5414 = AXIS2_PLACEMENT_3D ( 'NONE', #3527, #17487, #176 ) ;
#5415 = EDGE_CURVE ( 'NONE', #13797, #12800, #22235, .T. ) ;
#5416 = AXIS2_PLACEMENT_3D ( 'NONE', #826, #14790, #6102 ) ;
#5417 = VERTEX_POINT ( 'NONE', #22487 ) ;
#5418 = ORIENTED_EDGE ( 'NONE', *, *, #3860, .F. ) ;
#5419 = ORIENTED_EDGE ( 'NONE', *, *, #4728, .T. ) ;
#5420 = VERTEX_POINT ( 'NONE', #1850 ) ;
#5421 = LINE ( 'NONE', #1871, #6279 ) ;
#5422 = CARTESIAN_POINT ( 'NONE',  ( 22.41556111754670866, 20.62010838399688240, 58.66542762804075295 ) ) ;
#5423 = CARTESIAN_POINT ( 'NONE',  ( 4.407762377731845760, 40.00000000000000711, -51.31072002866562798 ) ) ;
#5424 = CARTESIAN_POINT ( 'NONE',  ( 5.708997389694868474, 39.99999999999998579, 51.95724523303017861 ) ) ;
#5425 = CIRCLE ( 'NONE', #9088, 49.99999999999998579 ) ;
#5426 = ORIENTED_EDGE ( 'NONE', *, *, #9879, .F. ) ;
#5427 = CYLINDRICAL_SURFACE ( 'NONE', #14558, 6.499999999999999112 ) ;
#5428 = CARTESIAN_POINT ( 'NONE',  ( -21.97438720605751783, 22.98755168577401520, 3.000000000000023537 ) ) ;
#5429 = ORIENTED_EDGE ( 'NONE', *, *, #4990, .T. ) ;
#5430 = CARTESIAN_POINT ( 'NONE',  ( -17.21639554191075305, 34.43961005730908198, -57.30688911148506293 ) ) ;
#5431 = AXIS2_PLACEMENT_3D ( 'NONE', #5323, #8763, #15735 ) ;
#5432 = CARTESIAN_POINT ( 'NONE',  ( -28.95348479018558407, 14.76298474240494940, 3.000000000000023537 ) ) ;
#5433 = EDGE_LOOP ( 'NONE', ( #8062, #555, #8875, #15349 ) ) ;
#5434 = CARTESIAN_POINT ( 'NONE',  ( 8.349099696857463115, 1.803277857257797656, 53.93591755799671006 ) ) ;
#5435 = ORIENTED_EDGE ( 'NONE', *, *, #15059, .F. ) ;
#5436 = CARTESIAN_POINT ( 'NONE',  ( 35.00000000000000000, 17.00000000000000000, 2.365113165210053967E-14 ) ) ;
#5437 = AXIS2_PLACEMENT_3D ( 'NONE', #11057, #4089, #16675 ) ;
#5438 = CARTESIAN_POINT ( 'NONE',  ( -1.575045212608098932, 39.94053886632075745, 50.55745523153140653 ) ) ;
#5439 = AXIS2_PLACEMENT_3D ( 'NONE', #22086, #20368, #6272 ) ;
#5440 = CARTESIAN_POINT ( 'NONE',  ( -9.689843208404443686, 39.33333333333332860, 54.54983754392751649 ) ) ;
#5441 = FILL_AREA_STYLE_COLOUR ( '', #1581 ) ;
#5442 = CARTESIAN_POINT ( 'NONE',  ( 15.91596560756312151, 32.12719615765404768, 56.91747558599882240 ) ) ;
#5443 = CARTESIAN_POINT ( 'NONE',  ( 1.110223024625156540E-13, -5.551115123125782702E-14, -6.999999999999950262 ) ) ;
#5444 = EDGE_CURVE ( 'NONE', #12921, #295, #22606, .T. ) ;
#5445 = EDGE_CURVE ( 'NONE', #10809, #15365, #5751, .T. ) ;
#5446 = CARTESIAN_POINT ( 'NONE',  ( -35.79662727779868447, 4.171001175319489107, -7.000000000000006217 ) ) ;
#5447 = AXIS2_PLACEMENT_3D ( 'NONE', #15801, #7106, #14074 ) ;
#5448 = ORIENTED_EDGE ( 'NONE', *, *, #13764, .F. ) ;
#5449 = ORIENTED_EDGE ( 'NONE', *, *, #2466, .F. ) ;
#5450 = EDGE_CURVE ( 'NONE', #9647, #9303, #12155, .T. ) ;
#5451 = ORIENTED_EDGE ( 'NONE', *, *, #3821, .F. ) ;
#5452 = AXIS2_PLACEMENT_3D ( 'NONE', #11104, #694, #21657 ) ;
#5453 = VERTEX_POINT ( 'NONE', #15466 ) ;
#5454 = CARTESIAN_POINT ( 'NONE',  ( 4.153395668489503478, -35.29097153256777375, -2.999999999999992006 ) ) ;
#5455 = FACE_OUTER_BOUND ( 'NONE', #20970, .T. ) ;
#5456 = DIRECTION ( 'NONE',  ( 0.000000000000000000, 0.000000000000000000, -1.000000000000000000 ) ) ;
#5457 = LINE ( 'NONE', #19214, #19709 ) ;
#5458 = CARTESIAN_POINT ( 'NONE',  ( 0.03495034244140499818, 39.99999280692916415, 48.76116143213860710 ) ) ;
#5459 = AXIS2_PLACEMENT_3D ( 'NONE', #15651, #5138, #17369 ) ;
#5460 = ORIENTED_EDGE ( 'NONE', *, *, #9253, .F. ) ;
#5461 = PLANE ( 'NONE',  #11914 ) ;
#5462 = CARTESIAN_POINT ( 'NONE',  ( 90.00000000000000000, 40.00000000000000000, -9.108981535246192915E-16 ) ) ;
#5463 = CIRCLE ( 'NONE', #18269, 34.90673715956759082 ) ;
#5464 = DIRECTION ( 'NONE',  ( 0.000000000000000000, 0.000000000000000000, 1.000000000000000000 ) ) ;
#5465 = CARTESIAN_POINT ( 'NONE',  ( -90.00000000000000000, 40.00000000000000711, -9.108981535246192915E-16 ) ) ;
#5466 = CARTESIAN_POINT ( 'NONE',  ( -8.215393105055671441, 1.749144060402865186, -56.08634520686066338 ) ) ;
#5467 = EDGE_CURVE ( 'NONE', #11128, #17574, #11238, .T. ) ;
#5468 = DIRECTION ( 'NONE',  ( -1.000000000000000000, -1.208970125616060101E-17, 6.505213034913038160E-19 ) ) ;
#5469 = FACE_BOUND ( 'NONE', #17372, .T. ) ;
#5470 = CARTESIAN_POINT ( 'NONE',  ( -30.48934413892778750, 16.99647590252656570, 2.999999999999999112 ) ) ;
#5471 = DIRECTION ( 'NONE',  ( 0.000000000000000000, 0.000000000000000000, -1.000000000000000000 ) ) ;
#5472 = VERTEX_POINT ( 'NONE', #15582 ) ;
#5473 = ORIENTED_EDGE ( 'NONE', *, *, #1803, .F. ) ;
#5474 = CIRCLE ( 'NONE', #16448, 2.500000000000002220 ) ;
#5475 = ORIENTED_EDGE ( 'NONE', *, *, #10128, .F. ) ;
#5476 = CARTESIAN_POINT ( 'NONE',  ( 5.770190843054305851, -4.767707482279640807, -49.21533144468782695 ) ) ;
#5477 = FACE_OUTER_BOUND ( 'NONE', #11545, .T. ) ;
#5478 = EDGE_CURVE ( 'NONE', #19994, #19216, #7609, .T. ) ;
#5479 = AXIS2_PLACEMENT_3D ( 'NONE', #5730, #19381, #10636 ) ;
#5480 = DIRECTION ( 'NONE',  ( 1.000000000000000000, 0.000000000000000000, 0.000000000000000000 ) ) ;
#5481 = CARTESIAN_POINT ( 'NONE',  ( -24.24871130596430291, 13.99999999999962341, -4.999999999999984013 ) ) ;
#5482 = DIRECTION ( 'NONE',  ( -1.000000000000000000, 0.000000000000000000, 0.000000000000000000 ) ) ;
#5483 = LINE ( 'NONE', #3770, #20780 ) ;
#5484 = CARTESIAN_POINT ( 'NONE',  ( -14.68506606271061443, 23.08193591670982059, -45.68712064066588852 ) ) ;
#5485 = EDGE_CURVE ( 'NONE', #19292, #6464, #22250, .T. ) ;
#5486 = VERTEX_POINT ( 'NONE', #15358 ) ;
#5487 = DIRECTION ( 'NONE',  ( -0.000000000000000000, 1.000000000000000000, -0.000000000000000000 ) ) ;
#5488 = DIRECTION ( 'NONE',  ( -0.000000000000000000, -0.000000000000000000, -1.000000000000000000 ) ) ;
#5489 = CARTESIAN_POINT ( 'NONE',  ( -13.00000000000000178, 20.00000000000000000, -11.32475165290611407 ) ) ;
#5490 = CARTESIAN_POINT ( 'NONE',  ( 35.00000000000000711, 2.142135623730931471, 50.00000000000000711 ) ) ;
#5491 = EDGE_LOOP ( 'NONE', ( #11037, #12057, #20420, #21919 ) ) ;
#5492 = CARTESIAN_POINT ( 'NONE',  ( -5.999999999999998224, 20.00000000000000000, 5.999999999999999112 ) ) ;
#5493 = CARTESIAN_POINT ( 'NONE',  ( 35.00000000000000000, 39.00000000000000711, 4.258610482196280173E-15 ) ) ;
#5494 = CIRCLE ( 'NONE', #9883, 2.500000000000002220 ) ;
#5495 = EDGE_CURVE ( 'NONE', #5750, #1187, #8997, .T. ) ;
#5496 = EDGE_LOOP ( 'NONE', ( #9868, #6218, #10357, #19825 ) ) ;
#5497 = EDGE_CURVE ( 'NONE', #4768, #6508, #13084, .T. ) ;
#5498 = ORIENTED_EDGE ( 'NONE', *, *, #18889, .F. ) ;
#5499 = DIRECTION ( 'NONE',  ( 0.000000000000000000, -1.000000000000000000, 0.000000000000000000 ) ) ;
#5500 = DIRECTION ( 'NONE',  ( 6.505213034913038160E-19, 3.903127820947822896E-18, 1.000000000000000000 ) ) ;
#5501 = DIRECTION ( 'NONE',  ( 0.000000000000000000, 0.000000000000000000, 1.000000000000000000 ) ) ;
#5502 = DIRECTION ( 'NONE',  ( 0.000000000000000000, 0.000000000000000000, 1.000000000000000000 ) ) ;
#5503 = ORIENTED_EDGE ( 'NONE', *, *, #17511, .T. ) ;
#5504 = DIRECTION ( 'NONE',  ( -1.000000000000000000, 1.530638361156006492E-16, 0.000000000000000000 ) ) ;
#5505 = DIRECTION ( 'NONE',  ( 1.000000000000000000, 0.000000000000000000, 0.000000000000000000 ) ) ;
#5506 = EDGE_LOOP ( 'NONE', ( #2812, #6535, #8458, #6349 ) ) ;
#5507 = CARTESIAN_POINT ( 'NONE',  ( 16.23964334364511686, 4.495128156857200352, -56.99255277661108465 ) ) ;
#5508 = CIRCLE ( 'NONE', #2600, 20.00000000000002132 ) ;
#5509 = DIRECTION ( 'NONE',  ( 0.000000000000000000, 0.000000000000000000, -1.000000000000000000 ) ) ;
#5510 = ORIENTED_EDGE ( 'NONE', *, *, #8922, .F. ) ;
#5511 = CARTESIAN_POINT ( 'NONE',  ( -1.387778780781445676E-14, 20.00000000000000000, -98.00000000000000000 ) ) ;
#5512 = CARTESIAN_POINT ( 'NONE',  ( -1.387778780781445676E-14, 20.00000000000000000, -102.0000000000000142 ) ) ;
#5513 = DIRECTION ( 'NONE',  ( -0.000000000000000000, 1.000000000000000000, -0.000000000000000000 ) ) ;
#5514 = ORIENTED_EDGE ( 'NONE', *, *, #4878, .F. ) ;
#5515 = LINE ( 'NONE', #7350, #10525 ) ;
#5516 = DIRECTION ( 'NONE',  ( -0.000000000000000000, -1.000000000000000000, -0.000000000000000000 ) ) ;
#5517 = CARTESIAN_POINT ( 'NONE',  ( -5.004946378181865718, 0.5943096879531011290, 54.03132084814318858 ) ) ;
#5518 = EDGE_CURVE ( 'NONE', #4344, #353, #17541, .T. ) ;
#5519 = ORIENTED_EDGE ( 'NONE', *, *, #9290, .T. ) ;
#5520 = ORIENTED_EDGE ( 'NONE', *, *, #3105, .T. ) ;
#5521 = ORIENTED_EDGE ( 'NONE', *, *, #11835, .F. ) ;
#5522 = EDGE_CURVE ( 'NONE', #14674, #11380, #7909, .T. ) ;
#5523 = ORIENTED_EDGE ( 'NONE', *, *, #11051, .F. ) ;
#5524 = CARTESIAN_POINT ( 'NONE',  ( 27.01645732367882857, 17.86915608785644238, -6.999999999999985789 ) ) ;
#5525 = CARTESIAN_POINT ( 'NONE',  ( 8.115805981708332340, 39.55796044940698408, -53.89994356748307780 ) ) ;
#5526 = CARTESIAN_POINT ( 'NONE',  ( 6.043799192484581084, 40.00000000000000000, 52.11526431830142059 ) ) ;
#5527 = ORIENTED_EDGE ( 'NONE', *, *, #22501, .T. ) ;
#5528 = CARTESIAN_POINT ( 'NONE',  ( -21.05198877411783442, 30.13956425491229396, -2.800654218530457484 ) ) ;
#5529 = CYLINDRICAL_SURFACE ( 'NONE', #9801, 6.499999999999999112 ) ;
#5530 = ORIENTED_EDGE ( 'NONE', *, *, #520, .T. ) ;
#5531 = LINE ( 'NONE', #19519, #21496 ) ;
#5532 = DIRECTION ( 'NONE',  ( 0.000000000000000000, 1.000000000000000000, 0.000000000000000000 ) ) ;
#5533 = AXIS2_PLACEMENT_3D ( 'NONE', #20308, #16862, #20192 ) ;
#5534 = LINE ( 'NONE', #3829, #245 ) ;
#5535 = CARTESIAN_POINT ( 'NONE',  ( -10.00000000000000888, 2.999999999999836131, -4.999999999999948486 ) ) ;
#5536 = ORIENTED_EDGE ( 'NONE', *, *, #3492, .F. ) ;
#5537 = DIRECTION ( 'NONE',  ( -0.000000000000000000, -1.000000000000000000, -0.000000000000000000 ) ) ;
#5538 = ADVANCED_FACE ( 'NONE', ( #13743 ), #5092, .T. ) ;
#5539 = DIRECTION ( 'NONE',  ( 0.000000000000000000, 0.000000000000000000, -1.000000000000000000 ) ) ;
#5540 = CARTESIAN_POINT ( 'NONE',  ( 16.99647590252670426, 30.48934413892764894, -2.999999999999971578 ) ) ;
#5541 = ADVANCED_FACE ( 'NONE', ( #19938 ), #8843, .F. ) ;
#5542 = DIRECTION ( 'NONE',  ( -0.000000000000000000, -1.000000000000000000, -0.000000000000000000 ) ) ;
#5543 = CARTESIAN_POINT ( 'NONE',  ( 19.93949378746059864, 21.61607484719042205, 60.60748883510628104 ) ) ;
#5544 = DIRECTION ( 'NONE',  ( -1.000000000000000000, -1.208970125616057944E-17, 0.000000000000000000 ) ) ;
#5545 = ADVANCED_FACE ( 'NONE', ( #4247 ), #18099, .F. ) ;
#5546 = CARTESIAN_POINT ( 'NONE',  ( -26.10969099697608797, -24.10368028608829505, -2.999999999999992006 ) ) ;
#5547 = EDGE_CURVE ( 'NONE', #4344, #15853, #13821, .T. ) ;
#5548 = ORIENTED_EDGE ( 'NONE', *, *, #12286, .F. ) ;
#5549 = AXIS2_PLACEMENT_3D ( 'NONE', #21339, #16287, #14216 ) ;
#5550 = EDGE_LOOP ( 'NONE', ( #19642, #18004, #2181, #19702 ) ) ;
#5551 = ORIENTED_EDGE ( 'NONE', *, *, #11758, .F. ) ;
#5552 = ORIENTED_EDGE ( 'NONE', *, *, #1245, .F. ) ;
#5553 = DIRECTION ( 'NONE',  ( -1.000000000000000000, 0.000000000000000000, 0.000000000000000000 ) ) ;
#5554 = DIRECTION ( 'NONE',  ( 0.000000000000000000, -1.000000000000000000, 0.000000000000000000 ) ) ;
#5555 = CARTESIAN_POINT ( 'NONE',  ( 5.833333333333328596, 33.81926995981416439, -40.61164310337066041 ) ) ;
#5556 = CARTESIAN_POINT ( 'NONE',  ( 0.000000000000000000, 30.00000000000000000, 0.000000000000000000 ) ) ;
#5557 = CARTESIAN_POINT ( 'NONE',  ( 1.107481208796976979, 39.99270069324596477, 49.57628741752042600 ) ) ;
#5558 = EDGE_CURVE ( 'NONE', #11380, #4189, #19728, .T. ) ;
#5559 = ADVANCED_FACE ( 'NONE', ( #17881 ), #5958, .F. ) ;
#5560 = VERTEX_POINT ( 'NONE', #5734 ) ;
#5561 = CARTESIAN_POINT ( 'NONE',  ( 10.60627602730578900, 0.5940385038083370040, -54.69850067894228118 ) ) ;
#5562 = CARTESIAN_POINT ( 'NONE',  ( -9.193775066140551289, 40.00000000000001421, -53.40447181574799629 ) ) ;
#5563 = LINE ( 'NONE', #2246, #16398 ) ;
#5564 = CARTESIAN_POINT ( 'NONE',  ( 13.56354382738798847, 2.142135623730931471, -56.03997097393683191 ) ) ;
#5565 = B_SPLINE_CURVE_WITH_KNOTS ( 'NONE', 3,
 ( #14730, #12561, #9142, #20030 ),
 .UNSPECIFIED., .F., .F.,
 ( 4, 4 ),
 ( 0.001893031756885345078, 0.003808480026563831368 ),
 .UNSPECIFIED. ) ;
#5566 = FILL_AREA_STYLE ('',( #2139 ) ) ;
#5567 = CIRCLE ( 'NONE', #9945, 2.524999999999999467 ) ;
#5568 = EDGE_CURVE ( 'NONE', #10048, #7926, #14127, .T. ) ;
#5569 = DIRECTION ( 'NONE',  ( -1.000000000000000000, -1.208970125616060717E-17, 0.000000000000000000 ) ) ;
#5570 = DIRECTION ( 'NONE',  ( -6.505213034913038160E-19, -3.903127820947822896E-18, -1.000000000000000000 ) ) ;
#5571 = CYLINDRICAL_SURFACE ( 'NONE', #17335, 15.00000000000000000 ) ;
#5572 = B_SPLINE_CURVE_WITH_KNOTS ( 'NONE', 3,
 ( #22188, #4996, #11527, #1207, #18978, #22416, #13448, #6262, #10021, #8205, #18857, #20470, #4778, #18743, #3049, #6709, #21972, #17013, #1323, #15285, #9692, #16679, #2826, #22312 ),
 .UNSPECIFIED., .F., .F.,
 ( 4, 2, 2, 2, 2, 2, 2, 2, 2, 2, 2, 4 ),
 ( 0.02614117015034102612, 0.02729036340605314401, 0.02843955666176526190, 0.03073794317318948727, 0.03188713642890159822, 0.03303632968461370917, 0.03533471619603793107, 0.03648390945175004896, 0.03763310270746215991, 0.03993148921888638181, 0.04222987573031060371, 0.04452826224173483255 ),
 .UNSPECIFIED. ) ;
#5573 = CARTESIAN_POINT ( 'NONE',  ( -35.00000000000000000, 40.00000000000000000, 51.00000000000002842 ) ) ;
#5574 = VERTEX_POINT ( 'NONE', #1247 ) ;
#5575 = EDGE_LOOP ( 'NONE', ( #9937, #7329, #9315 ) ) ;
#5576 = ORIENTED_EDGE ( 'NONE', *, *, #20522, .T. ) ;
#5577 = CONICAL_SURFACE ( 'NONE', #5946, 2.525000000000110489, 0.7853981633971014453 ) ;
#5578 = DIRECTION ( 'NONE',  ( 1.000000000000000000, 0.000000000000000000, 0.000000000000000000 ) ) ;
#5579 = VECTOR ( 'NONE', #11270, 1000.000000000000000 ) ;
#5580 = ADVANCED_FACE ( 'NONE', ( #6410 ), #10513, .T. ) ;
#5581 = CARTESIAN_POINT ( 'NONE',  ( -35.00000000000000000, 6.999999999999999112, 41.00000000000002132 ) ) ;
#5582 = DIRECTION ( 'NONE',  ( 0.000000000000000000, -1.000000000000000000, 0.000000000000000000 ) ) ;
#5583 = CARTESIAN_POINT ( 'NONE',  ( -14.04165170564761311, 5.752764646445623242, 58.83649392397244071 ) ) ;
#5584 = CARTESIAN_POINT ( 'NONE',  ( -15.06716847275263937, 33.15945890355343550, -59.19951139074274238 ) ) ;
#5585 = DIRECTION ( 'NONE',  ( -0.000000000000000000, -0.000000000000000000, -1.000000000000000000 ) ) ;
#5586 = ORIENTED_EDGE ( 'NONE', *, *, #17086, .F. ) ;
#5587 = DIRECTION ( 'NONE',  ( 0.000000000000000000, -1.000000000000000000, 0.000000000000000000 ) ) ;
#5588 = DIRECTION ( 'NONE',  ( -0.000000000000000000, 1.000000000000000000, -0.000000000000000000 ) ) ;
#5589 = CARTESIAN_POINT ( 'NONE',  ( -7.538500903810553488, 38.52938254314624800, -55.92181088654619714 ) ) ;
#5590 = DIRECTION ( 'NONE',  ( 0.000000000000000000, 0.000000000000000000, 1.000000000000000000 ) ) ;
#5591 = DIRECTION ( 'NONE',  ( 0.000000000000000000, -1.000000000000000000, 0.000000000000000000 ) ) ;
#5592 = ORIENTED_EDGE ( 'NONE', *, *, #17408, .T. ) ;
#5593 = DIRECTION ( 'NONE',  ( 6.505213034913038160E-19, 3.903127820947822896E-18, 1.000000000000000000 ) ) ;
#5594 = DIRECTION ( 'NONE',  ( 0.8391477167891896460, 0.3845457931435838361, -0.3846500258456542198 ) ) ;
#5595 = CONICAL_SURFACE ( 'NONE', #8535, 33.99999999999999289, 1.308996938995745873 ) ;
#5596 = AXIS2_PLACEMENT_3D ( 'NONE', #362, #7353, #14321 ) ;
#5597 = EDGE_CURVE ( 'NONE', #22687, #4837, #14537, .T. ) ;
#5598 = CARTESIAN_POINT ( 'NONE',  ( -42.50000000000000711, -12.00000000000000000, 47.50000000000000711 ) ) ;
#5599 = B_SPLINE_CURVE_WITH_KNOTS ( 'NONE', 3,
 ( #8952, #588, #5517, #244, #12602, #7578 ),
 .UNSPECIFIED., .F., .F.,
 ( 4, 2, 4 ),
 ( 0.000000000000000000, 0.004604358499702467140, 0.009208716999404934281 ),
 .UNSPECIFIED. ) ;
#5600 = EDGE_LOOP ( 'NONE', ( #17503, #10626, #9470, #219 ) ) ;
#5601 = EDGE_CURVE ( 'NONE', #13103, #22583, #12352, .T. ) ;
#5602 = AXIS2_PLACEMENT_3D ( 'NONE', #405, #4196, #12990 ) ;
#5603 = EDGE_LOOP ( 'NONE', ( #2360, #9910, #6653, #18837 ) ) ;
#5604 = CARTESIAN_POINT ( 'NONE',  ( -6.696867368503558448E-15, 0.000000000000000000, -48.73397172404479960 ) ) ;
#5605 = DIRECTION ( 'NONE',  ( -0.000000000000000000, 1.000000000000000000, -0.000000000000000000 ) ) ;
#5606 = VECTOR ( 'NONE', #1425, 1000.000000000000000 ) ;
#5607 = CYLINDRICAL_SURFACE ( 'NONE', #16426, 0.9999999999999974465 ) ;
#5608 = ORIENTED_EDGE ( 'NONE', *, *, #2035, .F. ) ;
#5609 = DIRECTION ( 'NONE',  ( 0.000000000000000000, 0.000000000000000000, -1.000000000000000000 ) ) ;
#5610 = VECTOR ( 'NONE', #3443, 1000.000000000000000 ) ;
#5611 = CARTESIAN_POINT ( 'NONE',  ( -12.10743492717932313, 1.299801688895240837, -55.43551573823073397 ) ) ;
#5612 = EDGE_LOOP ( 'NONE', ( #4406, #14116, #16090, #19294 ) ) ;
#5613 = DIRECTION ( 'NONE',  ( -0.000000000000000000, -1.000000000000000000, -0.000000000000000000 ) ) ;
#5614 = CARTESIAN_POINT ( 'NONE',  ( -22.00000000000001421, 20.00000000000000000, -100.0000000000000000 ) ) ;
#5615 = AXIS2_PLACEMENT_3D ( 'NONE', #15789, #8820, #8477 ) ;
#5616 = CARTESIAN_POINT ( 'NONE',  ( 21.93942599038054908, 24.73590942562830008, -58.56147853046843466 ) ) ;
#5617 = CYLINDRICAL_SURFACE ( 'NONE', #8129, 27.99999999999999645 ) ;
#5618 = ORIENTED_EDGE ( 'NONE', *, *, #3841, .T. ) ;
#5619 = DIRECTION ( 'NONE',  ( 1.000000000000000000, 0.000000000000000000, 0.000000000000000000 ) ) ;
#5620 = CARTESIAN_POINT ( 'NONE',  ( -13.85640646055073333, 1.500000000000008216, -8.000000000000493827 ) ) ;
#5621 = CARTESIAN_POINT ( 'NONE',  ( -6.264962414979408756, 39.74816732676359976, -52.94809031933390742 ) ) ;
#5622 = ORIENTED_EDGE ( 'NONE', *, *, #15348, .F. ) ;
#5623 = AXIS2_PLACEMENT_3D ( 'NONE', #12093, #12312, #10248 ) ;
#5624 =( BOUNDED_SURFACE ( )  B_SPLINE_SURFACE ( 3, 2, ( 
 ( #3590, #19613, #19397 ),
 ( #3923, #1752, #1860 ),
 ( #5304, #10549, #8841 ),
 ( #2305, #13050, #2655 ),
 ( #5864, #8036, #16508 ),
 ( #9630, #2544, #16277 ) ),
 .UNSPECIFIED., .F., .F., .F. ) 
 B_SPLINE_SURFACE_WITH_KNOTS ( ( 4, 2, 4 ),
 ( 3, 3 ),
 ( 0.000000000000000000, 0.002858401832368546482, 0.005716803664737092963 ),
 ( 0.000000000000000000, 1.000000000000000000 ),
 .UNSPECIFIED. ) 
 GEOMETRIC_REPRESENTATION_ITEM ( )  RATIONAL_B_SPLINE_SURFACE ( (
 ( 1.000000000000000000, 0.6290213284793376713, 1.000000000000000000),
 ( 1.000000000000000000, 0.6455195629501313537, 1.000000000000000000),
 ( 1.000000000000000000, 0.6615687397059663022, 1.000000000000000000),
 ( 1.000000000000000000, 0.6920701670989356513, 1.000000000000000000),
 ( 1.000000000000000000, 0.7065285139746015908, 1.000000000000000000),
 ( 1.000000000000000000, 0.7200096751079870794, 1.000000000000000000) ) ) 
 REPRESENTATION_ITEM ( '' )  SURFACE ( )  );
#5625 = DIRECTION ( 'NONE',  ( 1.000000000000000000, 0.000000000000000000, 0.000000000000000000 ) ) ;
#5626 = CARTESIAN_POINT ( 'NONE',  ( -16.56444186175087907, 26.79308242454872513, -2.999999999999992450 ) ) ;
#5627 = ADVANCED_FACE ( 'NONE', ( #16943 ), #11680, .F. ) ;
#5628 = VECTOR ( 'NONE', #880, 1000.000000000000000 ) ;
#5629 = AXIS2_PLACEMENT_3D ( 'NONE', #16504, #2539, #9957 ) ;
#5630 = VERTEX_POINT ( 'NONE', #11344 ) ;
#5631 = EDGE_CURVE ( 'NONE', #11797, #10749, #20415, .T. ) ;
#5632 = EDGE_LOOP ( 'NONE', ( #3691, #20196, #6618, #20738 ) ) ;
#5633 = VERTEX_POINT ( 'NONE', #9853 ) ;
#5634 = ORIENTED_EDGE ( 'NONE', *, *, #3759, .F. ) ;
#5635 = DIRECTION ( 'NONE',  ( 1.000000000000000000, 1.208970125616063182E-17, 0.000000000000000000 ) ) ;
#5636 = DIRECTION ( 'NONE',  ( 0.000000000000000000, -1.000000000000000000, 0.000000000000000000 ) ) ;
#5637 = APPLICATION_CONTEXT ( 'automotive_design' ) ;
#5638 = FACE_OUTER_BOUND ( 'NONE', #14565, .T. ) ;
#5639 = CARTESIAN_POINT ( 'NONE',  ( 7.325661905094778881, 40.00000000000000711, 52.68655283169726999 ) ) ;
#5640 = AXIS2_PLACEMENT_3D ( 'NONE', #5187, #13631, #20648 ) ;
#5641 = ORIENTED_EDGE ( 'NONE', *, *, #2995, .F. ) ;
#5642 = CARTESIAN_POINT ( 'NONE',  ( 3.330669073875469621E-13, -1.110223024625156540E-13, -2.999999999999971578 ) ) ;
#5643 = DIRECTION ( 'NONE',  ( 0.000000000000000000, 0.000000000000000000, -1.000000000000000000 ) ) ;
#5644 = ORIENTED_EDGE ( 'NONE', *, *, #5957, .F. ) ;
#5645 = CARTESIAN_POINT ( 'NONE',  ( 20.54749497201924058, -29.74882400976400376, 2.932969818539067131 ) ) ;
#5646 = CARTESIAN_POINT ( 'NONE',  ( -22.30616949375637503, 22.91984106672850174, -58.64191913087365293 ) ) ;
#5647 = CARTESIAN_POINT ( 'NONE',  ( 35.92356703407504170, 4.104166344908929176, 2.932460736555814407 ) ) ;
#5648 = VERTEX_POINT ( 'NONE', #21776 ) ;
#5649 = EDGE_CURVE ( 'NONE', #10179, #5750, #13030, .T. ) ;
#5650 = CARTESIAN_POINT ( 'NONE',  ( 22.12933039895921894, 3.000000000000003109, 2.710061364035962525E-15 ) ) ;
#5651 = EDGE_LOOP ( 'NONE', ( #1175, #11374, #16172, #18724 ) ) ;
#5652 = FACE_OUTER_BOUND ( 'NONE', #19669, .T. ) ;
#5653 = CARTESIAN_POINT ( 'NONE',  ( 25.00000000000000355, 20.00000000000000000, 16.49999999999999289 ) ) ;
#5654 = VECTOR ( 'NONE', #13416, 1000.000000000000000 ) ;
#5655 = CARTESIAN_POINT ( 'NONE',  ( 1.591932335265033587E-15, -4.923002280079127832E-27, 50.50395615645412306 ) ) ;
#5656 = VERTEX_POINT ( 'NONE', #18676 ) ;
#5657 = CARTESIAN_POINT ( 'NONE',  ( 90.00000000000000000, 40.00000000000000711, -9.108981535246192915E-16 ) ) ;
#5658 = CARTESIAN_POINT ( 'NONE',  ( 20.00401474702854543, 19.84140115762890133, 58.14847693657672778 ) ) ;
#5659 = DIRECTION ( 'NONE',  ( -6.505213034913038160E-19, -3.903127820947822896E-18, -1.000000000000000000 ) ) ;
#5660 = EDGE_CURVE ( 'NONE', #2593, #22272, #7987, .T. ) ;
#5661 = EDGE_CURVE ( 'NONE', #5124, #19660, #4328, .T. ) ;
#5662 = CARTESIAN_POINT ( 'NONE',  ( 9.998533603140314696, 40.00000000000000000, -54.54288842742649734 ) ) ;
#5663 = AXIS2_PLACEMENT_3D ( 'NONE', #11881, #6286, #22441 ) ;
#5664 = VERTEX_POINT ( 'NONE', #9617 ) ;
#5665 = VECTOR ( 'NONE', #677, 1000.000000000000000 ) ;
#5666 = ORIENTED_EDGE ( 'NONE', *, *, #3240, .T. ) ;
#5667 = EDGE_CURVE ( 'NONE', #16668, #13519, #11627, .T. ) ;
#5668 = ORIENTED_EDGE ( 'NONE', *, *, #11189, .T. ) ;
#5669 = ORIENTED_EDGE ( 'NONE', *, *, #13612, .T. ) ;
#5670 = CYLINDRICAL_SURFACE ( 'NONE', #11792, 60.00000000000000000 ) ;
#5671 = DIRECTION ( 'NONE',  ( 1.000000000000000000, -1.084202172485464991E-16, 0.000000000000000000 ) ) ;
#5672 = CARTESIAN_POINT ( 'NONE',  ( -11.99999999999999289, 28.19616000222403684, 0.000000000000000000 ) ) ;
#5673 = EDGE_CURVE ( 'NONE', #15024, #8904, #22644, .T. ) ;
#5674 = ORIENTED_EDGE ( 'NONE', *, *, #14947, .F. ) ;
#5675 = CARTESIAN_POINT ( 'NONE',  ( 17.66631876130925249, -31.41173278719244877, 2.999999999999995559 ) ) ;
#5676 = AXIS2_PLACEMENT_3D ( 'NONE', #21640, #21757, #21410 ) ;
#5677 = VECTOR ( 'NONE', #1365, 1000.000000000000000 ) ;
#5678 = ADVANCED_FACE ( 'NONE', ( #11220 ), #4474, .F. ) ;
#5679 = VERTEX_POINT ( 'NONE', #7788 ) ;
#5680 = LINE ( 'NONE', #14137, #19244 ) ;
#5681 = FACE_OUTER_BOUND ( 'NONE', #10634, .T. ) ;
#5682 = FACE_OUTER_BOUND ( 'NONE', #13070, .T. ) ;
#5683 = CARTESIAN_POINT ( 'NONE',  ( -20.00000000000002132, 20.48974789854086254, -60.62177826491083721 ) ) ;
#5684 = AXIS2_PLACEMENT_3D ( 'NONE', #20645, #1514, #10427 ) ;
#5685 = DIRECTION ( 'NONE',  ( -1.000000000000000000, 1.301042606982605814E-16, 0.000000000000000000 ) ) ;
#5686 = EDGE_CURVE ( 'NONE', #7816, #19292, #11451, .T. ) ;
#5687 = EDGE_CURVE ( 'NONE', #21104, #668, #8339, .T. ) ;
#5688 = CARTESIAN_POINT ( 'NONE',  ( -1.268121568164027657, 39.97056933375353083, 50.22305475358200511 ) ) ;
#5689 = DIRECTION ( 'NONE',  ( 0.000000000000000000, 0.000000000000000000, 1.000000000000000000 ) ) ;
#5690 = AXIS2_PLACEMENT_3D ( 'NONE', #1152, #20410, #11908 ) ;
#5691 = EDGE_CURVE ( 'NONE', #5386, #20516, #20795, .T. ) ;
#5692 = ORIENTED_EDGE ( 'NONE', *, *, #18498, .T. ) ;
#5693 = AXIS2_PLACEMENT_3D ( 'NONE', #16797, #11294, #12994 ) ;
#5694 = ORIENTED_EDGE ( 'NONE', *, *, #4553, .T. ) ;
#5695 = EDGE_CURVE ( 'NONE', #16203, #19009, #1026, .T. ) ;
#5696 = AXIS2_PLACEMENT_3D ( 'NONE', #9097, #10793, #14580 ) ;
#5697 = ORIENTED_EDGE ( 'NONE', *, *, #612, .T. ) ;
#5698 = CIRCLE ( 'NONE', #19963, 34.90673715956759082 ) ;
#5699 = CARTESIAN_POINT ( 'NONE',  ( 2.602085213965210642E-15, 5.025303850726727362, 0.000000000000000000 ) ) ;
#5700 = DIRECTION ( 'NONE',  ( 0.000000000000000000, 1.000000000000000000, -0.000000000000000000 ) ) ;
#5701 = CYLINDRICAL_SURFACE ( 'NONE', #12448, 10.00000000000000000 ) ;
#5702 = CARTESIAN_POINT ( 'NONE',  ( 35.00000000000001421, -1.000000000000028644, 1.540743955509788682E-30 ) ) ;
#5703 = CARTESIAN_POINT ( 'NONE',  ( -19.74829075628835895, 16.81150045999882892, 60.56179516789185868 ) ) ;
#5704 = CARTESIAN_POINT ( 'NONE',  ( -11.93214024655444838, 36.05624711372846036, -58.01435237789498700 ) ) ;
#5705 = AXIS2_PLACEMENT_3D ( 'NONE', #4318, #18507, #11170 ) ;
#5706 = CARTESIAN_POINT ( 'NONE',  ( -14.67611967928926475, 31.67162468655990182, -2.999999999999971578 ) ) ;
#5707 = AXIS2_PLACEMENT_3D ( 'NONE', #1040, #13603, #8474 ) ;
#5708 = ORIENTED_EDGE ( 'NONE', *, *, #10301, .F. ) ;
#5709 = FACE_OUTER_BOUND ( 'NONE', #12121, .T. ) ;
#5710 = DIRECTION ( 'NONE',  ( -1.000000000000000000, 0.000000000000000000, 0.000000000000000000 ) ) ;
#5711 = CARTESIAN_POINT ( 'NONE',  ( -34.84717828836173936, 6.955395936296730142, -3.000000000000011990 ) ) ;
#5712 = CARTESIAN_POINT ( 'NONE',  ( 0.000000000000000000, 9.999999999999998224, 0.000000000000000000 ) ) ;
#5713 = DIRECTION ( 'NONE',  ( -0.000000000000000000, -0.000000000000000000, 1.000000000000000000 ) ) ;
#5714 = AXIS2_PLACEMENT_3D ( 'NONE', #9156, #14178, #5718 ) ;
#5715 = ORIENTED_EDGE ( 'NONE', *, *, #17671, .F. ) ;
#5716 = CARTESIAN_POINT ( 'NONE',  ( -9.999999999999758415, -3.000000000000169198, -4.999999999999984013 ) ) ;
#5717 = FACE_OUTER_BOUND ( 'NONE', #6893, .T. ) ;
#5718 = DIRECTION ( 'NONE',  ( 1.000000000000000000, 0.000000000000000000, 0.000000000000000000 ) ) ;
#5719 = EDGE_CURVE ( 'NONE', #21713, #5723, #13440, .T. ) ;
#5720 = CARTESIAN_POINT ( 'NONE',  ( 42.50000000000000711, -12.00000000000000000, -45.40000000000000568 ) ) ;
#5721 = AXIS2_PLACEMENT_3D ( 'NONE', #1958, #12381, #15917 ) ;
#5722 = CIRCLE ( 'NONE', #22190, 2.499999999999998668 ) ;
#5723 = VERTEX_POINT ( 'NONE', #5261 ) ;
#5724 = CIRCLE ( 'NONE', #18535, 6.499999999999999112 ) ;
#5725 = CARTESIAN_POINT ( 'NONE',  ( -18.65063509461096913, 12.49999999999990052, -5.000000000000004441 ) ) ;
#5726 = EDGE_CURVE ( 'NONE', #877, #5417, #19643, .T. ) ;
#5727 = ORIENTED_EDGE ( 'NONE', *, *, #14097, .F. ) ;
#5728 = CARTESIAN_POINT ( 'NONE',  ( 2.999999999999999556, 22.00000000000000000, 6.485281374238567764 ) ) ;
#5729 = VECTOR ( 'NONE', #19562, 1000.000000000000000 ) ;
#5730 = CARTESIAN_POINT ( 'NONE',  ( -42.50000000000000711, -12.00000000000000000, -47.50000000000000000 ) ) ;
#5731 = DIRECTION ( 'NONE',  ( -6.505213034913038160E-19, -3.903127820947822896E-18, -1.000000000000000000 ) ) ;
#5732 = VERTEX_POINT ( 'NONE', #22456 ) ;
#5733 = CARTESIAN_POINT ( 'NONE',  ( 11.98978967046198996, 34.10919265018070945, 2.932969818539058249 ) ) ;
#5734 = CARTESIAN_POINT ( 'NONE',  ( -30.57187188083528540, -7.711478842616581453, 3.000000000000023537 ) ) ;
#5735 = ORIENTED_EDGE ( 'NONE', *, *, #5379, .F. ) ;
#5736 = CARTESIAN_POINT ( 'NONE',  ( 6.070730550691044947, 31.88709182564705813, 2.999999999999995559 ) ) ;
#5737 = CARTESIAN_POINT ( 'NONE',  ( 3.330669073875469621E-13, -1.110223024625156540E-13, -2.999999999999971578 ) ) ;
#5738 = CARTESIAN_POINT ( 'NONE',  ( -27.84804035626035912, 24.75236754129145211, -2.999999999999995559 ) ) ;
#5739 = CARTESIAN_POINT ( 'NONE',  ( -18.83615802559775076, 32.14641817400173807, -6.999999999999950262 ) ) ;
#5740 = ORIENTED_EDGE ( 'NONE', *, *, #4183, .F. ) ;
#5741 = DIRECTION ( 'NONE',  ( 0.000000000000000000, -1.000000000000000000, 0.000000000000000000 ) ) ;
#5742 = CARTESIAN_POINT ( 'NONE',  ( -9.062586715433361917, 2.130694986431509452, 54.31128890271796195 ) ) ;
#5743 = CARTESIAN_POINT ( 'NONE',  ( -0.3255759151790424410, 39.99938828955776415, -48.98576778550931010 ) ) ;
#5744 = AXIS2_PLACEMENT_3D ( 'NONE', #12715, #810, #7794 ) ;
#5745 = EDGE_LOOP ( 'NONE', ( #3226, #16056, #12963, #12339 ) ) ;
#5746 = CARTESIAN_POINT ( 'NONE',  ( 35.00000000000001421, 5.000000000000000000, -10.00000000000000000 ) ) ;
#5747 = EDGE_CURVE ( 'NONE', #22237, #18105, #6636, .T. ) ;
#5748 = DIRECTION ( 'NONE',  ( 0.4166911066143264564, 0.000000000000000000, -0.9090481404571091328 ) ) ;
#5749 = CARTESIAN_POINT ( 'NONE',  ( 42.50000000000000000, 10.00000000000000000, 47.49999999999999289 ) ) ;
#5750 = VERTEX_POINT ( 'NONE', #3087 ) ;
#5751 = CIRCLE ( 'NONE', #8682, 19.11328065563151668 ) ;
#5752 = ORIENTED_EDGE ( 'NONE', *, *, #8040, .F. ) ;
#5753 = AXIS2_PLACEMENT_3D ( 'NONE', #1624, #8832, #17084 ) ;
#5754 = ORIENTED_EDGE ( 'NONE', *, *, #8717, .T. ) ;
#5755 =( NAMED_UNIT ( * ) SI_UNIT ( $, .STERADIAN. ) SOLID_ANGLE_UNIT ( ) );
#5756 = CIRCLE ( 'NONE', #643, 17.00000000000000711 ) ;
#5757 = EDGE_LOOP ( 'NONE', ( #19066, #16404 ) ) ;
#5758 = PLANE ( 'NONE',  #21652 ) ;
#5759 = DIRECTION ( 'NONE',  ( -1.000000000000000000, 0.000000000000000000, 0.000000000000000000 ) ) ;
#5760 = CARTESIAN_POINT ( 'NONE',  ( 15.12081897056669000, -33.51030287062373247, -2.000000000000005329 ) ) ;
#5761 = DIRECTION ( 'NONE',  ( -1.000000000000000000, 0.000000000000000000, 0.000000000000000000 ) ) ;
#5762 = ORIENTED_EDGE ( 'NONE', *, *, #18578, .T. ) ;
#5763 = DIRECTION ( 'NONE',  ( 0.000000000000000000, 0.000000000000000000, 1.000000000000000000 ) ) ;
#5764 = LINE ( 'NONE', #11253, #20042 ) ;
#5765 = ORIENTED_EDGE ( 'NONE', *, *, #7700, .T. ) ;
#5766 = CARTESIAN_POINT ( 'NONE',  ( -1.143118858956962969, 0.005001482714649774057, 49.65374274205655780 ) ) ;
#5767 = EDGE_CURVE ( 'NONE', #20460, #7282, #1363, .T. ) ;
#5768 = DIRECTION ( 'NONE',  ( 0.000000000000000000, 0.000000000000000000, 1.000000000000000000 ) ) ;
#5769 = CARTESIAN_POINT ( 'NONE',  ( -4.080045426412465481, 32.20238537491798780, 2.999999999999995559 ) ) ;
#5770 = ORIENTED_EDGE ( 'NONE', *, *, #11418, .F. ) ;
#5771 = DIRECTION ( 'NONE',  ( 0.000000000000000000, 0.000000000000000000, 1.000000000000000000 ) ) ;
#5772 = EDGE_LOOP ( 'NONE', ( #4067, #9159, #597 ) ) ;
#5773 = CARTESIAN_POINT ( 'NONE',  ( -42.49999999999996447, 7.000000000000000000, -47.50000000000000711 ) ) ;
#5774 = AXIS2_PLACEMENT_3D ( 'NONE', #9311, #14445, #21455 ) ;
#5775 = CARTESIAN_POINT ( 'NONE',  ( -33.51030287062352642, -15.12081897056683033, 2.800654218530502337 ) ) ;
#5776 = EDGE_CURVE ( 'NONE', #10413, #20463, #6888, .T. ) ;
#5777 = VERTEX_POINT ( 'NONE', #17390 ) ;
#5778 = AXIS2_PLACEMENT_3D ( 'NONE', #13039, #804, #4368 ) ;
#5779 = CARTESIAN_POINT ( 'NONE',  ( 17.96644252022819188, 11.16803817567472201, 57.57522208103243599 ) ) ;
#5780 = LINE ( 'NONE', #15964, #7778 ) ;
#5781 = CIRCLE ( 'NONE', #21513, 6.499999999999999112 ) ;
#5782 = LINE ( 'NONE', #12864, #3098 ) ;
#5783 = EDGE_LOOP ( 'NONE', ( #8667, #15668, #3669, #3541 ) ) ;
#5784 = ORIENTED_EDGE ( 'NONE', *, *, #6712, .F. ) ;
#5785 = EDGE_CURVE ( 'NONE', #5453, #20150, #18965, .T. ) ;
#5786 = AXIS2_PLACEMENT_3D ( 'NONE', #9334, #13503, #1380 ) ;
#5787 = ORIENTED_EDGE ( 'NONE', *, *, #10657, .T. ) ;
#5788 = ORIENTED_EDGE ( 'NONE', *, *, #6256, .F. ) ;
#5789 = DIRECTION ( 'NONE',  ( -1.000000000000000000, 1.301042606982605814E-16, 0.000000000000000000 ) ) ;
#5790 = VECTOR ( 'NONE', #17568, 1000.000000000000000 ) ;
#5791 = CARTESIAN_POINT ( 'NONE',  ( -10.95789470854538372, 39.14627205512025654, -55.00167764528740122 ) ) ;
#5792 = AXIS2_PLACEMENT_3D ( 'NONE', #1141, #8240, #6073 ) ;
#5793 = FACE_BOUND ( 'NONE', #19042, .T. ) ;
#5794 = CIRCLE ( 'NONE', #12008, 58.99999999999994316 ) ;
#5795 = ORIENTED_EDGE ( 'NONE', *, *, #18779, .F. ) ;
#5796 = CARTESIAN_POINT ( 'NONE',  ( 10.30713387248560231, 2.842164160679857332, 57.27491564205545416 ) ) ;
#5797 = CARTESIAN_POINT ( 'NONE',  ( 7.325260514639500961E-15, -4.648749848371387827, 45.43309249825157536 ) ) ;
#5798 = EDGE_CURVE ( 'NONE', #6084, #11772, #6509, .T. ) ;
#5799 = TOROIDAL_SURFACE ( 'NONE', #20804, 34.90673715956759082, 8.750000000000000000 ) ;
#5800 = ORIENTED_EDGE ( 'NONE', *, *, #14410, .F. ) ;
#5801 = CARTESIAN_POINT ( 'NONE',  ( 42.50000000000000711, -9.600000000000001421, 49.60000000000000853 ) ) ;
#5802 = DIRECTION ( 'NONE',  ( 0.000000000000000000, 0.000000000000000000, 1.000000000000000000 ) ) ;
#5803 = DIRECTION ( 'NONE',  ( -6.505213034913038160E-19, -3.903127820947822896E-18, -1.000000000000000000 ) ) ;
#5804 = AXIS2_PLACEMENT_3D ( 'NONE', #8668, #3525, #12106 ) ;
#5805 = DIRECTION ( 'NONE',  ( 6.505213034913038160E-19, 3.903127820947822896E-18, 1.000000000000000000 ) ) ;
#5806 = VECTOR ( 'NONE', #17418, 1000.000000000000000 ) ;
#5807 = AXIS2_PLACEMENT_3D ( 'NONE', #4565, #21747, #13132 ) ;
#5808 = CARTESIAN_POINT ( 'NONE',  ( -3.981170799216933176, 39.90684832978752183, 51.58237208215641090 ) ) ;
#5809 = CARTESIAN_POINT ( 'NONE',  ( 42.50000000000000000, 10.00000000000000000, 47.49999999999999289 ) ) ;
#5810 = CIRCLE ( 'NONE', #11664, 12.00000000000000000 ) ;
#5811 = VERTEX_POINT ( 'NONE', #15779 ) ;
#5812 = EDGE_LOOP ( 'NONE', ( #6401, #8899, #9786, #4982 ) ) ;
#5813 = EDGE_CURVE ( 'NONE', #862, #3734, #19017, .T. ) ;
#5814 = ORIENTED_EDGE ( 'NONE', *, *, #8846, .F. ) ;
#5815 = CARTESIAN_POINT ( 'NONE',  ( 32.75570538720803881, -15.02862401740803833, 2.999999999999995559 ) ) ;
#5816 = PRESENTATION_LAYER_ASSIGNMENT (  '', '', ( #9844 ) ) ;
#5817 = AXIS2_PLACEMENT_3D ( 'NONE', #8053, #2561, #7817 ) ;
#5818 = FACE_OUTER_BOUND ( 'NONE', #2469, .T. ) ;
#5819 = ADVANCED_FACE ( 'NONE', ( #5158 ), #6983, .T. ) ;
#5820 = ADVANCED_FACE ( 'NONE', ( #13939 ), #3551, .T. ) ;
#5821 = ADVANCED_FACE ( 'NONE', ( #19126 ), #7241, .T. ) ;
#5822 = DIRECTION ( 'NONE',  ( -1.000000000000000000, -1.208970125616046080E-17, 6.505213034913038160E-19 ) ) ;
#5823 = CYLINDRICAL_SURFACE ( 'NONE', #18624, 31.50000000000001421 ) ;
#5824 = CARTESIAN_POINT ( 'NONE',  ( -11.87139216507977224, 36.11857111619887206, -55.37976054165662987 ) ) ;
#5825 = FACE_OUTER_BOUND ( 'NONE', #16665, .T. ) ;
#5826 = DIRECTION ( 'NONE',  ( -0.000000000000000000, -1.000000000000000000, -0.000000000000000000 ) ) ;
#5827 = DIRECTION ( 'NONE',  ( 1.000000000000000000, 0.000000000000000000, 1.224646799147353207E-16 ) ) ;
#5828 = DIRECTION ( 'NONE',  ( 1.000000000000000000, 0.000000000000000000, 0.000000000000000000 ) ) ;
#5829 = PRODUCT ( 'ROTARY LOBE', 'ROTARY LOBE', '', ( #10300 ) ) ;
#5830 = EDGE_LOOP ( 'NONE', ( #7004, #17103, #16908, #20604 ) ) ;
#5831 = CARTESIAN_POINT ( 'NONE',  ( 35.00000000000058265, 26.00000000000000355, -55.00000000000076028 ) ) ;
#5832 = EDGE_CURVE ( 'NONE', #1767, #13224, #1711, .T. ) ;
#5833 = CARTESIAN_POINT ( 'NONE',  ( 21.65063509461093005, 12.50000000000006750, -5.000000000000004441 ) ) ;
#5834 = DIRECTION ( 'NONE',  ( 0.000000000000000000, -1.000000000000000000, 0.000000000000000000 ) ) ;
#5835 = DIRECTION ( 'NONE',  ( 0.000000000000000000, 0.000000000000000000, 1.000000000000000000 ) ) ;
#5836 = ORIENTED_EDGE ( 'NONE', *, *, #22331, .F. ) ;
#5837 = DIRECTION ( 'NONE',  ( -1.000000000000000000, -1.208970125616063490E-17, 0.000000000000000000 ) ) ;
#5838 = VERTEX_POINT ( 'NONE', #13714 ) ;
#5839 = CARTESIAN_POINT ( 'NONE',  ( -34.99999999999999289, 0.000000000000000000, -3.012171160963566127E-14 ) ) ;
#5840 = DIRECTION ( 'NONE',  ( 1.000000000000000000, -0.000000000000000000, 3.063596499322173499E-16 ) ) ;
#5841 = VERTEX_POINT ( 'NONE', #22579 ) ;
#5842 = CARTESIAN_POINT ( 'NONE',  ( 32.83234229683740324, -11.85401191286897316, 2.999999999999995559 ) ) ;
#5843 = CARTESIAN_POINT ( 'NONE',  ( 6.257506482006864879, 40.00000000000000000, -52.21447511918912454 ) ) ;
#5844 = VERTEX_POINT ( 'NONE', #4812 ) ;
#5845 = CARTESIAN_POINT ( 'NONE',  ( 0.6620738645431283320, 39.99747006418269279, -49.24250857139721660 ) ) ;
#5846 = CARTESIAN_POINT ( 'NONE',  ( 9.689843208404402830, 39.33333333333334991, 54.54983754392742412 ) ) ;
#5847 = AXIS2_PLACEMENT_3D ( 'NONE', #12613, #12294, #19299 ) ;
#5848 = LINE ( 'NONE', #14189, #21913 ) ;
#5849 = VERTEX_POINT ( 'NONE', #6869 ) ;
#5850 = CARTESIAN_POINT ( 'NONE',  ( 14.99999999999998579, 20.00000000000000000, 101.0000000000000568 ) ) ;
#5851 = CARTESIAN_POINT ( 'NONE',  ( -10.31465995609250186, 2.846668092512739001, -57.27881138849976139 ) ) ;
#5852 = ORIENTED_EDGE ( 'NONE', *, *, #2365, .F. ) ;
#5853 = CARTESIAN_POINT ( 'NONE',  ( -90.00000000000000000, 26.00000000000000355, -9.108981535246192915E-16 ) ) ;
#5854 = FACE_OUTER_BOUND ( 'NONE', #10443, .T. ) ;
#5855 = EDGE_CURVE ( 'NONE', #2582, #3905, #3227, .T. ) ;
#5856 = DIRECTION ( 'NONE',  ( 6.505213034913038160E-19, 3.903127820947822896E-18, 1.000000000000000000 ) ) ;
#5857 = ADVANCED_FACE ( 'NONE', ( #12023 ), #15673, .F. ) ;
#5858 = FACE_OUTER_BOUND ( 'NONE', #2819, .T. ) ;
#5859 = VERTEX_POINT ( 'NONE', #19361 ) ;
#5860 = CYLINDRICAL_SURFACE ( 'NONE', #19284, 20.00000000000000000 ) ;
#5861 = CARTESIAN_POINT ( 'NONE',  ( -11.05758567243163348, 3.294696707140393421, 55.18338768059884103 ) ) ;
#5862 = CARTESIAN_POINT ( 'NONE',  ( -0.1974767274569673714, 39.99977542932850127, -48.88709713040997684 ) ) ;
#5863 = ORIENTED_EDGE ( 'NONE', *, *, #10962, .T. ) ;
#5864 = CARTESIAN_POINT ( 'NONE',  ( 9.867969867544811535, 0.2954100743844931820, 54.30456930252214676 ) ) ;
#5865 = CIRCLE ( 'NONE', #19772, 19.11328065563152379 ) ;
#5866 = EDGE_CURVE ( 'NONE', #9501, #14814, #11077, .T. ) ;
#5867 = CARTESIAN_POINT ( 'NONE',  ( -9.852267639826644441, 31.31642578264289156, 43.21671877549179897 ) ) ;
#5868 = DIRECTION ( 'NONE',  ( -0.000000000000000000, -0.000000000000000000, 1.000000000000000000 ) ) ;
#5869 = CONICAL_SURFACE ( 'NONE', #9893, 57.00000000000002132, 0.7853981633974437271 ) ;
#5870 = EDGE_LOOP ( 'NONE', ( #21915, #4926, #10252, #8989 ) ) ;
#5871 = VERTEX_POINT ( 'NONE', #3665 ) ;
#5872 = ORIENTED_EDGE ( 'NONE', *, *, #10237, .F. ) ;
#5873 = DIRECTION ( 'NONE',  ( -0.006752834798041749097, -0.9999753815462444351, -0.001906704915093601974 ) ) ;
#5874 = VERTEX_POINT ( 'NONE', #16008 ) ;
#5875 = DIRECTION ( 'NONE',  ( 6.505213034913038160E-19, 3.903127820947822896E-18, 1.000000000000000000 ) ) ;
#5876 = CARTESIAN_POINT ( 'NONE',  ( -5.074925817841774212, 32.10132595304123981, -2.999999999999999112 ) ) ;
#5877 = DIRECTION ( 'NONE',  ( 0.000000000000000000, -1.000000000000000000, 0.000000000000000000 ) ) ;
#5878 = CARTESIAN_POINT ( 'NONE',  ( -12.99999999999980282, -2.516660498395516310, -105.0010000000000048 ) ) ;
#5879 = CARTESIAN_POINT ( 'NONE',  ( -42.50000000000000711, -9.600000000000001421, 49.60000000000000853 ) ) ;
#5880 = EDGE_LOOP ( 'NONE', ( #11231, #9186, #7970, #2543 ) ) ;
#5881 = DIRECTION ( 'NONE',  ( 0.000000000000000000, 0.000000000000000000, -1.000000000000000000 ) ) ;
#5882 = FACE_OUTER_BOUND ( 'NONE', #2007, .T. ) ;
#5883 = ORIENTED_EDGE ( 'NONE', *, *, #14368, .T. ) ;
#5884 = FACE_OUTER_BOUND ( 'NONE', #19623, .T. ) ;
#5885 = CARTESIAN_POINT ( 'NONE',  ( 4.456525674222657894E-15, 6.180736333215575584, 0.000000000000000000 ) ) ;
#5886 = ORIENTED_EDGE ( 'NONE', *, *, #13929, .T. ) ;
#5887 = FACE_OUTER_BOUND ( 'NONE', #20818, .T. ) ;
#5888 = ORIENTED_EDGE ( 'NONE', *, *, #14810, .F. ) ;
#5889 = CARTESIAN_POINT ( 'NONE',  ( 3.171143452058838186, 39.94219392501161536, 51.05053595446507586 ) ) ;
#5890 = CARTESIAN_POINT ( 'NONE',  ( 35.00000000000000000, -5.000000000000000000, 54.99999999999698019 ) ) ;
#5891 = EDGE_LOOP ( 'NONE', ( #22001, #12669 ) ) ;
#5892 = DIRECTION ( 'NONE',  ( 1.000000000000000000, 0.000000000000000000, -0.000000000000000000 ) ) ;
#5893 = CARTESIAN_POINT ( 'NONE',  ( 6.696867368503558448E-15, 39.00000000000000711, 48.73397172404481381 ) ) ;
#5894 = LINE ( 'NONE', #3958, #4864 ) ;
#5895 = CIRCLE ( 'NONE', #11742, 31.50000000000000711 ) ;
#5896 = VECTOR ( 'NONE', #19298, 1000.000000000000000 ) ;
#5897 = DIRECTION ( 'NONE',  ( 6.505213034913038160E-19, 3.903127820947822896E-18, 1.000000000000000000 ) ) ;
#5899 = ORIENTED_EDGE ( 'NONE', *, *, #17210, .T. ) ;
#5898 = ADVANCED_FACE ( 'NONE', ( #12676 ), #17622, .T. ) ;
#5900 = ORIENTED_EDGE ( 'NONE', *, *, #2829, .F. ) ;
#5901 = ORIENTED_EDGE ( 'NONE', *, *, #637, .F. ) ;
#5902 = ORIENTED_EDGE ( 'NONE', *, *, #16886, .F. ) ;
#5903 = DIRECTION ( 'NONE',  ( -0.000000000000000000, -1.000000000000000000, -0.000000000000000000 ) ) ;
#5904 = CARTESIAN_POINT ( 'NONE',  ( 13.85640646055118808, 1.500000000000004885, 7.999999999999710454 ) ) ;
#5905 = ADVANCED_FACE ( 'NONE', ( #4107 ), #17962, .T. ) ;
#5906 = CIRCLE ( 'NONE', #11394, 11.99999999999999822 ) ;
#5907 = CARTESIAN_POINT ( 'NONE',  ( -32.89999999999981384, 28.00000000000000000, 54.99999999999922551 ) ) ;
#5908 = ORIENTED_EDGE ( 'NONE', *, *, #5661, .T. ) ;
#5909 = CARTESIAN_POINT ( 'NONE',  ( 18.00000000000019185, -2.519513924556040635E-14, 4.999999999999993783 ) ) ;
#5910 = CARTESIAN_POINT ( 'NONE',  ( -35.00000000000000000, 7.000000000000000000, 2.365113165210053967E-14 ) ) ;
#5911 = ORIENTED_EDGE ( 'NONE', *, *, #16926, .F. ) ;
#5912 = DIRECTION ( 'NONE',  ( 8.659560562351929024E-17, -0.7071067811867928210, 0.7071067811863022134 ) ) ;
#5913 = LINE ( 'NONE', #12879, #7242 ) ;
#5914 = DIRECTION ( 'NONE',  ( -0.000000000000000000, 1.000000000000000000, -0.000000000000000000 ) ) ;
#5915 = DIRECTION ( 'NONE',  ( 0.000000000000000000, 1.000000000000000000, 0.000000000000000000 ) ) ;
#5916 = DIRECTION ( 'NONE',  ( -6.505213034913038160E-19, -3.903127820947822896E-18, -1.000000000000000000 ) ) ;
#5917 = VECTOR ( 'NONE', #19853, 1000.000000000000000 ) ;
#5918 = DIRECTION ( 'NONE',  ( -0.000000000000000000, 1.000000000000000000, -0.000000000000000000 ) ) ;
#5919 = DIRECTION ( 'NONE',  ( -0.9012767464701780806, -2.276634065091486700E-15, -0.4332438415859253267 ) ) ;
#5920 = ADVANCED_FACE ( 'NONE', ( #662 ), #5823, .T. ) ;
#5921 = VERTEX_POINT ( 'NONE', #10616 ) ;
#5922 = ORIENTED_EDGE ( 'NONE', *, *, #18266, .F. ) ;
#5923 = ORIENTED_EDGE ( 'NONE', *, *, #280, .T. ) ;
#5924 = ADVANCED_FACE ( 'NONE', ( #12348 ), #4001, .T. ) ;
#5925 = FACE_OUTER_BOUND ( 'NONE', #3204, .T. ) ;
#5926 = CARTESIAN_POINT ( 'NONE',  ( -3.469446951953614189E-14, -3.999999999999985345, 48.73397172404114031 ) ) ;
#5927 = VECTOR ( 'NONE', #19943, 1000.000000000000000 ) ;
#5928 = CARTESIAN_POINT ( 'NONE',  ( 6.775279300855725495, 38.82186504314601194, 55.41168644275258970 ) ) ;
#5929 = CARTESIAN_POINT ( 'NONE',  ( -10.60627602730584407, 0.5940385038083494385, -54.69850067894230250 ) ) ;
#5930 = CARTESIAN_POINT ( 'NONE',  ( -1.575019415474304463, 39.98856485926602744, -49.93405284605607619 ) ) ;
#5931 = CARTESIAN_POINT ( 'NONE',  ( -7.474202570535936729, 30.60042966911716178, -2.999999999999971578 ) ) ;
#5932 = CARTESIAN_POINT ( 'NONE',  ( -34.99999999999999289, -3.999999999999985345, -3.012171160963566127E-14 ) ) ;
#5933 = EDGE_CURVE ( 'NONE', #3830, #18499, #2509, .T. ) ;
#5934 = EDGE_LOOP ( 'NONE', ( #22485, #16323 ) ) ;
#5935 = DIRECTION ( 'NONE',  ( -6.505213034913038160E-19, -3.903127820947822896E-18, -1.000000000000000000 ) ) ;
#5936 = CARTESIAN_POINT ( 'NONE',  ( -0.1564864144765418241, 40.00000000000000711, -48.92140276528787268 ) ) ;
#5937 = CARTESIAN_POINT ( 'NONE',  ( 4.929203366568097207E-16, 30.00000000000000355, -4.025000000000000355 ) ) ;
#5938 = CARTESIAN_POINT ( 'NONE',  ( 29.36548507648051398, 13.83143812983095344, -2.999999999999971578 ) ) ;
#5939 = ORIENTED_EDGE ( 'NONE', *, *, #14145, .T. ) ;
#5940 = VERTEX_POINT ( 'NONE', #15888 ) ;
#5941 = DIRECTION ( 'NONE',  ( -1.000000000000000000, 1.020425574104004122E-16, 0.000000000000000000 ) ) ;
#5942 = DIRECTION ( 'NONE',  ( -1.000000000000000000, -0.000000000000000000, -0.000000000000000000 ) ) ;
#5943 = EDGE_CURVE ( 'NONE', #10163, #7430, #12235, .T. ) ;
#5944 = EDGE_CURVE ( 'NONE', #18599, #16070, #17128, .T. ) ;
#5945 = VECTOR ( 'NONE', #5582, 1000.000000000000000 ) ;
#5946 = AXIS2_PLACEMENT_3D ( 'NONE', #16091, #19545, #400 ) ;
#5947 = VERTEX_POINT ( 'NONE', #2160 ) ;
#5948 = CARTESIAN_POINT ( 'NONE',  ( -36.54278193890294091, -4.025500340002652777, 2.800654218530481465 ) ) ;
#5949 = EDGE_CURVE ( 'NONE', #11275, #11481, #9145, .T. ) ;
#5950 = DIRECTION ( 'NONE',  ( -6.505213034913038160E-19, -3.903127820947822896E-18, -1.000000000000000000 ) ) ;
#5951 = ORIENTED_EDGE ( 'NONE', *, *, #13007, .F. ) ;
#5952 = CARTESIAN_POINT ( 'NONE',  ( 1.044236013776834060, 39.99351860983329487, -49.52927844032964089 ) ) ;
#5953 = FACE_OUTER_BOUND ( 'NONE', #1080, .T. ) ;
#5954 = CARTESIAN_POINT ( 'NONE',  ( -35.00000000000000000, -5.000000000000000000, 1.387778780781445676E-14 ) ) ;
#5955 = EDGE_LOOP ( 'NONE', ( #4087, #11962, #5551, #11753, #4287 ) ) ;
#5956 = DIRECTION ( 'NONE',  ( 1.000000000000000000, 1.208970125616053475E-17, 0.000000000000000000 ) ) ;
#5957 = EDGE_CURVE ( 'NONE', #2840, #4080, #14512, .T. ) ;
#5958 = CYLINDRICAL_SURFACE ( 'NONE', #15278, 18.00000000000000000 ) ;
#5959 = ORIENTED_EDGE ( 'NONE', *, *, #18442, .F. ) ;
#5960 = LINE ( 'NONE', #6194, #13055 ) ;
#5961 = CARTESIAN_POINT ( 'NONE',  ( -90.00000000000000000, 40.00000000000000711, -2.525000000000000355 ) ) ;
#5962 = DIRECTION ( 'NONE',  ( 6.505213034913038160E-19, 3.903127820947822896E-18, 1.000000000000000000 ) ) ;
#5963 = EDGE_CURVE ( 'NONE', #16920, #6360, #18189, .T. ) ;
#5964 = ORIENTED_EDGE ( 'NONE', *, *, #17873, .T. ) ;
#5965 = CARTESIAN_POINT ( 'NONE',  ( -12.10743492717950609, 1.299801688895098506, 55.43551573823082634 ) ) ;
#5966 = DIRECTION ( 'NONE',  ( -0.4332438415860033198, 0.000000000000000000, 0.9012767464701406661 ) ) ;
#5967 = AXIS2_PLACEMENT_3D ( 'NONE', #21598, #9211, #19653 ) ;
#5968 = ORIENTED_EDGE ( 'NONE', *, *, #9129, .T. ) ;
#5969 = CYLINDRICAL_SURFACE ( 'NONE', #19242, 31.50000000000000000 ) ;
#5970 = DIRECTION ( 'NONE',  ( 1.296372316667914327E-16, 1.000000000000000000, -0.000000000000000000 ) ) ;
#5972 = EDGE_CURVE ( 'NONE', #3909, #16743, #21985, .T. ) ;
#5971 = ORIENTED_EDGE ( 'NONE', *, *, #3335, .T. ) ;
#5973 = AXIS2_PLACEMENT_3D ( 'NONE', #6839, #17477, #5230 ) ;
#5974 = ORIENTED_EDGE ( 'NONE', *, *, #13218, .F. ) ;
#5975 = ORIENTED_EDGE ( 'NONE', *, *, #12491, .F. ) ;
#5976 = CIRCLE ( 'NONE', #16595, 18.00000000000000000 ) ;
#5977 = DIRECTION ( 'NONE',  ( 0.9999707308947706208, -0.006759637085566803406, 0.003583944788867206733 ) ) ;
#5978 = UNCERTAINTY_MEASURE_WITH_UNIT (LENGTH_MEASURE( 1.000000000000000082E-05 ), #6729, 'distance_accuracy_value', 'NONE');
#5979 = CIRCLE ( 'NONE', #16577, 34.90673715956759082 ) ;
#5980 = VERTEX_POINT ( 'NONE', #6385 ) ;
#5981 = CARTESIAN_POINT ( 'NONE',  ( 19.92971843794354214, 21.94076660514457444, -60.60536071356334276 ) ) ;
#5982 = CARTESIAN_POINT ( 'NONE',  ( 17.09029715894955359, -27.64365646977279312, -7.000000000000006217 ) ) ;
#5983 = DIRECTION ( 'NONE',  ( -0.000000000000000000, -1.000000000000000000, -0.000000000000000000 ) ) ;
#5984 = CARTESIAN_POINT ( 'NONE',  ( 2.854018578421813982E-15, -6.180736333215565814, 0.000000000000000000 ) ) ;
#5985 = CARTESIAN_POINT ( 'NONE',  ( -22.97438720605733664, 22.98755168577407204, -2.999999999999971578 ) ) ;
#5986 = VERTEX_POINT ( 'NONE', #7760 ) ;
#5987 = CARTESIAN_POINT ( 'NONE',  ( -13.85640646055084702, 1.500000000000008216, 7.999999999999705125 ) ) ;
#5988 = DIRECTION ( 'NONE',  ( 0.000000000000000000, -1.000000000000000000, 0.000000000000000000 ) ) ;
#5989 = ORIENTED_EDGE ( 'NONE', *, *, #1104, .F. ) ;
#5990 = CARTESIAN_POINT ( 'NONE',  ( 1.011722470948207109, 35.51751788033340773, -3.000000000000015543 ) ) ;
#5991 = CIRCLE ( 'NONE', #14753, 19.11328065563151668 ) ;
#5992 = CARTESIAN_POINT ( 'NONE',  ( 19.80871821058214266, 17.21148610482000407, -60.57629886234794014 ) ) ;
#5993 = ORIENTED_EDGE ( 'NONE', *, *, #2653, .F. ) ;
#5994 = CARTESIAN_POINT ( 'NONE',  ( -9.952189117650851458, 40.00000000000000000, -53.64426396172072486 ) ) ;
#5995 = AXIS2_PLACEMENT_3D ( 'NONE', #20480, #17138, #16915 ) ;
#5996 = DIRECTION ( 'NONE',  ( 0.000000000000000000, 0.000000000000000000, 1.000000000000000000 ) ) ;
#5997 = ORIENTED_EDGE ( 'NONE', *, *, #15433, .F. ) ;
#5998 = CARTESIAN_POINT ( 'NONE',  ( -1.265314100866710527E-14, 40.00000000000000000, 48.73397172404481381 ) ) ;
#5999 = LINE ( 'NONE', #7490, #7179 ) ;
#6000 = DIRECTION ( 'NONE',  ( -0.000000000000000000, 1.000000000000000000, -0.000000000000000000 ) ) ;
#6001 = ORIENTED_EDGE ( 'NONE', *, *, #7330, .F. ) ;
#6002 = CARTESIAN_POINT ( 'NONE',  ( 31.11077005834439291, -4.936596639065371050, -6.999999999999950262 ) ) ;
#6003 = CIRCLE ( 'NONE', #19531, 17.00000000000000000 ) ;
#6004 = CARTESIAN_POINT ( 'NONE',  ( 15.91103418227299215, 35.86133518681679533, 56.88632568426859137 ) ) ;
#6005 = FACE_OUTER_BOUND ( 'NONE', #14704, .T. ) ;
#6006 = AXIS2_PLACEMENT_3D ( 'NONE', #21992, #17123, #16708 ) ;
#6007 = AXIS2_PLACEMENT_3D ( 'NONE', #1261, #22015, #20411 ) ;
#6008 = DIRECTION ( 'NONE',  ( -0.000000000000000000, -1.000000000000000000, -0.000000000000000000 ) ) ;
#6010 = EDGE_CURVE ( 'NONE', #7482, #5420, #19910, .T. ) ;
#6009 = ORIENTED_EDGE ( 'NONE', *, *, #14053, .F. ) ;
#6011 = ORIENTED_EDGE ( 'NONE', *, *, #13624, .T. ) ;
#6012 = CIRCLE ( 'NONE', #15868, 2.500000000000002220 ) ;
#6013 = ORIENTED_EDGE ( 'NONE', *, *, #16529, .F. ) ;
#6014 = EDGE_LOOP ( 'NONE', ( #13694, #2827, #8705, #18362 ) ) ;
#6015 = DIRECTION ( 'NONE',  ( -6.505213034913038160E-19, -3.903127820947822896E-18, -1.000000000000000000 ) ) ;
#6016 = DIRECTION ( 'NONE',  ( 0.000000000000000000, 0.000000000000000000, -1.000000000000000000 ) ) ;
#6017 = PRODUCT_DEFINITION_SHAPE ( 'NONE', 'NONE',  #22700 ) ;
#6018 = CONICAL_SURFACE ( 'NONE', #15139, 2.524999999999999467, 0.7853981633974482790 ) ;
#6019 = ADVANCED_FACE ( 'NONE', ( #16471 ), #11283, .F. ) ;
#6020 = ORIENTED_EDGE ( 'NONE', *, *, #14495, .F. ) ;
#6021 = DIRECTION ( 'NONE',  ( 1.000000000000000000, 0.000000000000000000, 0.000000000000000000 ) ) ;
#6022 = CARTESIAN_POINT ( 'NONE',  ( -34.99999999999999289, 5.000000000000000000, -3.012171160963566127E-14 ) ) ;
#6023 = CIRCLE ( 'NONE', #16612, 2.999999999999999112 ) ;
#6024 = ORIENTED_EDGE ( 'NONE', *, *, #15419, .T. ) ;
#6025 = CARTESIAN_POINT ( 'NONE',  ( -18.22261011550273224, -31.92986134326242365, -2.800654218530485018 ) ) ;
#6026 = DIRECTION ( 'NONE',  ( -0.000000000000000000, -1.000000000000000000, -0.000000000000000000 ) ) ;
#6027 = CARTESIAN_POINT ( 'NONE',  ( 90.00000000000000000, 40.00000000000000000, -9.108981535246192915E-16 ) ) ;
#6028 = EDGE_CURVE ( 'NONE', #2421, #11565, #13451, .T. ) ;
#6029 = CIRCLE ( 'NONE', #18836, 16.49999999999999645 ) ;
#6030 = DIRECTION ( 'NONE',  ( 0.000000000000000000, 1.000000000000000000, 0.000000000000000000 ) ) ;
#6031 = AXIS2_PLACEMENT_3D ( 'NONE', #18768, #8016, #6287 ) ;
#6032 = EDGE_CURVE ( 'NONE', #3715, #14229, #7623, .T. ) ;
#6033 = CARTESIAN_POINT ( 'NONE',  ( -5.340789179572045242, 39.27722415257186839, 54.28402915905244441 ) ) ;
#6034 = CARTESIAN_POINT ( 'NONE',  ( -32.35999952201586183, 1.423424233832598640, 2.999999999999995559 ) ) ;
#6035 = ORIENTED_EDGE ( 'NONE', *, *, #4936, .F. ) ;
#6036 = EDGE_LOOP ( 'NONE', ( #20811, #10587, #15420, #2760 ) ) ;
#6037 = AXIS2_PLACEMENT_3D ( 'NONE', #9836, #16706, #1126 ) ;
#6038 = VERTEX_POINT ( 'NONE', #18410 ) ;
#6039 = DIRECTION ( 'NONE',  ( 0.000000000000000000, 0.000000000000000000, 1.000000000000000000 ) ) ;
#6040 = CIRCLE ( 'NONE', #7500, 2.999999999999999112 ) ;
#6041 = DIRECTION ( 'NONE',  ( 1.445602896647339410E-16, 0.000000000000000000, 1.000000000000000000 ) ) ;
#6042 = AXIS2_PLACEMENT_3D ( 'NONE', #1401, #8059, #15362 ) ;
#6043 = CARTESIAN_POINT ( 'NONE',  ( 7.928388824789353251, 38.36675580713608014, 56.15749817958555923 ) ) ;
#6044 = CARTESIAN_POINT ( 'NONE',  ( -12.82970538955584772, 1.687462484003157126, -55.75926248610263514 ) ) ;
#6045 = CARTESIAN_POINT ( 'NONE',  ( -8.123074520535881859, 39.63120893085925189, -53.85470301846236651 ) ) ;
#6046 = CARTESIAN_POINT ( 'NONE',  ( 5.999999999999999112, -40.00000000000000000, -6.000000000000000000 ) ) ;
#6047 = EDGE_CURVE ( 'NONE', #14638, #9888, #291, .T. ) ;
#6048 = LINE ( 'NONE', #13015, #15559 ) ;
#6049 = ORIENTED_EDGE ( 'NONE', *, *, #2294, .F. ) ;
#6050 = CARTESIAN_POINT ( 'NONE',  ( -11.68090480754633553, 3.765577839755389622, 57.90797000640144176 ) ) ;
#6051 = DIRECTION ( 'NONE',  ( -0.000000000000000000, 1.000000000000000000, -0.000000000000000000 ) ) ;
#6052 = CARTESIAN_POINT ( 'NONE',  ( 14.76298474240531000, 28.95348479018561250, -7.000000000000006217 ) ) ;
#6053 = AXIS2_PLACEMENT_3D ( 'NONE', #2920, #17098, #1414 ) ;
#6054 = DIRECTION ( 'NONE',  ( 0.000000000000000000, 0.000000000000000000, 1.000000000000000000 ) ) ;
#6055 = EDGE_CURVE ( 'NONE', #18413, #16878, #19458, .T. ) ;
#6056 = ORIENTED_EDGE ( 'NONE', *, *, #11607, .T. ) ;
#6057 = ORIENTED_EDGE ( 'NONE', *, *, #9831, .T. ) ;
#6058 = CARTESIAN_POINT ( 'NONE',  ( 35.16985127952396084, 10.70799354677376414, 2.800654218530485018 ) ) ;
#6059 = CIRCLE ( 'NONE', #6854, 19.11328065563150957 ) ;
#6060 = VECTOR ( 'NONE', #21273, 1000.000000000000000 ) ;
#6061 = VERTEX_POINT ( 'NONE', #1543 ) ;
#6062 = DIRECTION ( 'NONE',  ( 0.000000000000000000, -1.000000000000000000, 0.000000000000000000 ) ) ;
#6063 = ADVANCED_FACE ( 'NONE', ( #2730 ), #18531, .T. ) ;
#6064 = DIRECTION ( 'NONE',  ( 6.505213034913038160E-19, 3.903127820947822896E-18, 1.000000000000000000 ) ) ;
#6065 = AXIS2_PLACEMENT_3D ( 'NONE', #12034, #19029, #16854 ) ;
#6066 = CIRCLE ( 'NONE', #3153, 34.90673715956759082 ) ;
#6067 = VERTEX_POINT ( 'NONE', #8002 ) ;
#6068 = CARTESIAN_POINT ( 'NONE',  ( 1.568459684872858473, 13.32608676515186730, 8.880481854261104147 ) ) ;
#6069 = CIRCLE ( 'NONE', #2043, 19.11328065563150957 ) ;
#6070 = CARTESIAN_POINT ( 'NONE',  ( 11.51194040401120056, 39.05862814753015044, 55.21283662269279091 ) ) ;
#6071 = ADVANCED_BREP_SHAPE_REPRESENTATION ( '', ( #18432, #18273 ), #1444 ) ;
#6072 = DIRECTION ( 'NONE',  ( 0.000000000000000000, -1.000000000000000000, 0.000000000000000000 ) ) ;
#6073 = DIRECTION ( 'NONE',  ( -1.000000000000000000, -1.208970125616046080E-17, 6.505213034913038160E-19 ) ) ;
#6074 = EDGE_CURVE ( 'NONE', #22110, #12599, #4343, .T. ) ;
#6076 = ADVANCED_FACE ( 'NONE', ( #1120 ), #18966, .F. ) ;
#6075 = FACE_OUTER_BOUND ( 'NONE', #11465, .T. ) ;
#6077 = CARTESIAN_POINT ( 'NONE',  ( -3.182710733240893486, 40.00000000000000711, 50.65274140376491374 ) ) ;
#6078 = AXIS2_PLACEMENT_3D ( 'NONE', #1576, #8455, #5148 ) ;
#6079 = DIRECTION ( 'NONE',  ( 0.000000000000000000, 0.000000000000000000, 1.000000000000000000 ) ) ;
#6080 = ORIENTED_EDGE ( 'NONE', *, *, #8804, .F. ) ;
#6081 = CYLINDRICAL_SURFACE ( 'NONE', #22209, 36.76383501243555685 ) ;
#6082 = CARTESIAN_POINT ( 'NONE',  ( 42.50000000000000711, -9.600000000000001421, 45.00000000000000711 ) ) ;
#6083 = DIRECTION ( 'NONE',  ( 0.000000000000000000, 0.000000000000000000, -1.000000000000000000 ) ) ;
#6084 = VERTEX_POINT ( 'NONE', #11967 ) ;
#6085 = CARTESIAN_POINT ( 'NONE',  ( 42.49999999999998579, 7.000000000000000000, -47.49999999999997868 ) ) ;
#6086 = APPLICATION_CONTEXT ( 'automotive_design' ) ;
#6087 = CARTESIAN_POINT ( 'NONE',  ( -9.579024991656975629, 31.54842267267896716, 43.05667825653220149 ) ) ;
#6088 = CARTESIAN_POINT ( 'NONE',  ( -48.93401015228422324, 7.000000000000000000, -46.57614213197970088 ) ) ;
#6089 = CIRCLE ( 'NONE', #13752, 2.500000000000002220 ) ;
#6090 = CIRCLE ( 'NONE', #18894, 8.999999999999966249 ) ;
#6091 = CIRCLE ( 'NONE', #8655, 19.11328065563152379 ) ;
#6092 = VERTEX_POINT ( 'NONE', #3276 ) ;
#6093 = VECTOR ( 'NONE', #9580, 1000.000000000000000 ) ;
#6094 = EDGE_CURVE ( 'NONE', #3823, #18686, #18303, .T. ) ;
#6095 = ORIENTED_EDGE ( 'NONE', *, *, #11836, .T. ) ;
#6096 = CARTESIAN_POINT ( 'NONE',  ( 188.3424255147120334, 176.4349250857161451, -11.51647599436479297 ) ) ;
#6097 = VERTEX_POINT ( 'NONE', #2619 ) ;
#6098 = CARTESIAN_POINT ( 'NONE',  ( 19.98183132229265269, 20.98212305896295149, 60.61750244562277601 ) ) ;
#6099 = CARTESIAN_POINT ( 'NONE',  ( -4.295527433237782828E-15, -1.236374842841486021, 48.24164917503448180 ) ) ;
#6100 = CYLINDRICAL_SURFACE ( 'NONE', #11363, 2.500000000000002220 ) ;
#6101 = CARTESIAN_POINT ( 'NONE',  ( 12.24744603029285273, 40.00000000000000000, 54.43639671998466412 ) ) ;
#6102 = DIRECTION ( 'NONE',  ( 0.000000000000000000, 0.000000000000000000, 1.000000000000000000 ) ) ;
#6103 = EDGE_LOOP ( 'NONE', ( #1898, #252, #6115, #10136 ) ) ;
#6104 = CARTESIAN_POINT ( 'NONE',  ( -15.00428685838175724, 32.89708536800382888, 2.932460736555835279 ) ) ;
#6105 = CARTESIAN_POINT ( 'NONE',  ( 22.28024240313503057, 22.26748298433264850, 3.000000000000023537 ) ) ;
#6106 = VERTEX_POINT ( 'NONE', #9592 ) ;
#6107 = ADVANCED_FACE ( 'NONE', ( #886 ), #7879, .T. ) ;
#6108 = CIRCLE ( 'NONE', #9770, 34.90673715956759082 ) ;
#6109 = EDGE_CURVE ( 'NONE', #8183, #2221, #14228, .T. ) ;
#6110 = CARTESIAN_POINT ( 'NONE',  ( -21.43973101033765261, 13.38729130222877650, -58.44776001661259812 ) ) ;
#6111 = DIRECTION ( 'NONE',  ( 1.768737661780273138E-15, 0.000000000000000000, 1.000000000000000000 ) ) ;
#6112 = ORIENTED_EDGE ( 'NONE', *, *, #13920, .F. ) ;
#6113 = CARTESIAN_POINT ( 'NONE',  ( 35.00000000000000000, 17.00000000000000000, -16.99999999999997868 ) ) ;
#6114 = CARTESIAN_POINT ( 'NONE',  ( 0.000000000000000000, 30.00000000000000000, -2.000000000000000000 ) ) ;
#6115 = ORIENTED_EDGE ( 'NONE', *, *, #19164, .T. ) ;
#6116 = CARTESIAN_POINT ( 'NONE',  ( -1.437422297277388872E-14, 40.00000000000000000, 48.73397172404481381 ) ) ;
#6117 = DIRECTION ( 'NONE',  ( -0.000000000000000000, -1.000000000000000000, -0.000000000000000000 ) ) ;
#6118 = CARTESIAN_POINT ( 'NONE',  ( -3.230019253414518669E-15, -0.1273124286837649666, -49.60950288446434087 ) ) ;
#6119 = CIRCLE ( 'NONE', #17763, 59.99999999999700862 ) ;
#6120 = EDGE_LOOP ( 'NONE', ( #8541, #17114 ) ) ;
#6121 = CARTESIAN_POINT ( 'NONE',  ( 13.73196689449483721, 34.57679379660663699, 56.13071196757302772 ) ) ;
#6122 = EDGE_CURVE ( 'NONE', #20378, #16159, #7397, .T. ) ;
#6123 = DIRECTION ( 'NONE',  ( -0.9898477157360406897, 0.000000000000000000, 0.1421319796954317316 ) ) ;
#6124 = CARTESIAN_POINT ( 'NONE',  ( 6.696867368504048330E-15, 5.000000000000000888, 38.73397172404480671 ) ) ;
#6125 = PLANE ( 'NONE',  #2727 ) ;
#6126 = AXIS2_PLACEMENT_3D ( 'NONE', #456, #4135, #4037 ) ;
#6127 = AXIS2_PLACEMENT_3D ( 'NONE', #8350, #1136, #6522 ) ;
#6128 = ORIENTED_EDGE ( 'NONE', *, *, #3298, .T. ) ;
#6129 = ORIENTED_EDGE ( 'NONE', *, *, #15717, .T. ) ;
#6130 = ORIENTED_EDGE ( 'NONE', *, *, #11304, .T. ) ;
#6131 = VERTEX_POINT ( 'NONE', #10795 ) ;
#6132 = CARTESIAN_POINT ( 'NONE',  ( -8.331955809010631597, 38.18181818181817988, -56.36098470834072316 ) ) ;
#6133 = TOROIDAL_SURFACE ( 'NONE', #11980, 34.90673715956759082, 8.750000000000000000 ) ;
#6134 = CIRCLE ( 'NONE', #5040, 2.524999999999999467 ) ;
#6135 = ORIENTED_EDGE ( 'NONE', *, *, #621, .T. ) ;
#6136 = CARTESIAN_POINT ( 'NONE',  ( -9.999999999999980460, -3.000000000000002665, 4.999999999999997335 ) ) ;
#6137 = LINE ( 'NONE', #9121, #8186 ) ;
#6138 = ORIENTED_EDGE ( 'NONE', *, *, #7212, .T. ) ;
#6139 = CARTESIAN_POINT ( 'NONE',  ( 2.673152730111972630, 14.43024452475228614, 8.612623190900158932 ) ) ;
#6140 = AXIS2_PLACEMENT_3D ( 'NONE', #6220, #9767, #13405 ) ;
#6141 = ORIENTED_EDGE ( 'NONE', *, *, #1987, .T. ) ;
#6142 = FACE_OUTER_BOUND ( 'NONE', #12733, .T. ) ;
#6143 = CIRCLE ( 'NONE', #15281, 1.000000000000000888 ) ;
#6144 = CARTESIAN_POINT ( 'NONE',  ( 0.7921581640149154557, 24.99916066339285692, 8.999720221271109821 ) ) ;
#6145 = DIRECTION ( 'NONE',  ( 0.000000000000000000, 0.000000000000000000, 1.000000000000000000 ) ) ;
#6146 = CARTESIAN_POINT ( 'NONE',  ( -0.4445462163336120764, 39.99884035387562875, 49.07689293423401011 ) ) ;
#6147 = EDGE_CURVE ( 'NONE', #15662, #20449, #21896, .T. ) ;
#6148 = ADVANCED_FACE ( 'NONE', ( #17345 ), #21244, .F. ) ;
#6149 = CARTESIAN_POINT ( 'NONE',  ( -34.99999999999999289, 1.000000000000044187, 9.999999999999971578 ) ) ;
#6150 = CARTESIAN_POINT ( 'NONE',  ( -6.450249579240430187, 39.75604022694633954, 53.02614836873388526 ) ) ;
#6151 = AXIS2_PLACEMENT_3D ( 'NONE', #1274, #22258, #1163 ) ;
#6152 = EDGE_CURVE ( 'NONE', #17751, #14282, #11641, .T. ) ;
#6153 = DIRECTION ( 'NONE',  ( 1.296372316667914327E-16, 1.000000000000000000, -0.000000000000000000 ) ) ;
#6154 = ORIENTED_EDGE ( 'NONE', *, *, #22279, .F. ) ;
#6155 = AXIS2_PLACEMENT_3D ( 'NONE', #12265, #6665, #8386 ) ;
#6156 = ORIENTED_EDGE ( 'NONE', *, *, #7339, .F. ) ;
#6157 = VECTOR ( 'NONE', #22307, 1000.000000000000000 ) ;
#6158 = CIRCLE ( 'NONE', #2872, 9.000000000000003553 ) ;
#6159 = EDGE_LOOP ( 'NONE', ( #18517, #19538, #7255, #22299 ) ) ;
#6160 = CARTESIAN_POINT ( 'NONE',  ( -20.11496009237101745, 10.03305173526369209, 58.12476682723770693 ) ) ;
#6161 = LINE ( 'NONE', #2259, #5628 ) ;
#6162 = DIRECTION ( 'NONE',  ( 0.000000000000000000, 1.000000000000000000, 0.000000000000000000 ) ) ;
#6163 = ADVANCED_FACE ( 'NONE', ( #19524 ), #6524, .F. ) ;
#6164 = CARTESIAN_POINT ( 'NONE',  ( 0.000000000000000000, 0.000000000000000000, 0.000000000000000000 ) ) ;
#6165 = VECTOR ( 'NONE', #21643, 1000.000000000000000 ) ;
#6166 = CARTESIAN_POINT ( 'NONE',  ( 3.581684221278998451E-14, -0.5379438610623193950, 48.80684069443805839 ) ) ;
#6167 = DIRECTION ( 'NONE',  ( -0.000000000000000000, -1.000000000000000000, -0.000000000000000000 ) ) ;
#6168 = CARTESIAN_POINT ( 'NONE',  ( -8.957567394277941020, 39.56957037178317904, -54.21303306609684114 ) ) ;
#6169 = FACE_OUTER_BOUND ( 'NONE', #4061, .T. ) ;
#6170 = AXIS2_PLACEMENT_3D ( 'NONE', #3038, #20343, #4766 ) ;
#6171 = AXIS2_PLACEMENT_3D ( 'NONE', #14392, #16354, #198 ) ;
#6172 = VERTEX_POINT ( 'NONE', #3499 ) ;
#6173 = CARTESIAN_POINT ( 'NONE',  ( -2.546974693918181654, 39.84782899243123921, -51.61921092574151970 ) ) ;
#6174 = FACE_OUTER_BOUND ( 'NONE', #7029, .T. ) ;
#6175 = FACE_OUTER_BOUND ( 'NONE', #22032, .T. ) ;
#6176 = VECTOR ( 'NONE', #5288, 1000.000000000000000 ) ;
#6177 = VERTEX_POINT ( 'NONE', #1884 ) ;
#6178 = CARTESIAN_POINT ( 'NONE',  ( 22.98755168577445929, 22.97438720605740770, -6.999999999999950262 ) ) ;
#6179 = CARTESIAN_POINT ( 'NONE',  ( -34.99999999999999289, 0.000000000000000000, -58.99999999999702993 ) ) ;
#6180 = DIRECTION ( 'NONE',  ( -1.000000000000000000, -0.000000000000000000, -0.000000000000000000 ) ) ;
#6181 = VECTOR ( 'NONE', #1565, 1000.000000000000000 ) ;
#6182 = VECTOR ( 'NONE', #19271, 1000.000000000000000 ) ;
#6183 = ORIENTED_EDGE ( 'NONE', *, *, #15884, .T. ) ;
#6184 = ADVANCED_FACE ( 'NONE', ( #5110 ), #265, .T. ) ;
#6185 = DIRECTION ( 'NONE',  ( 0.000000000000000000, 0.000000000000000000, 1.000000000000000000 ) ) ;
#6186 = CARTESIAN_POINT ( 'NONE',  ( 4.873427793009105002, 40.00000000000000000, -51.54633075627398853 ) ) ;
#6187 = VERTEX_POINT ( 'NONE', #8643 ) ;
#6188 = CARTESIAN_POINT ( 'NONE',  ( 0.2719366648872892367, 39.99956353068301240, -48.94448570199384108 ) ) ;
#6189 = EDGE_CURVE ( 'NONE', #4950, #17173, #13897, .T. ) ;
#6190 = CARTESIAN_POINT ( 'NONE',  ( 9.952189117650823036, 40.00000000000000000, 53.64426396172073197 ) ) ;
#6191 = DIRECTION ( 'NONE',  ( -1.000000000000000000, 1.445602896647339410E-16, 0.000000000000000000 ) ) ;
#6192 = DIRECTION ( 'NONE',  ( 0.000000000000000000, 0.000000000000000000, 1.000000000000000000 ) ) ;
#6193 = B_SPLINE_CURVE_WITH_KNOTS ( 'NONE', 3,
 ( #20619, #20742, #5051, #19025 ),
 .UNSPECIFIED., .F., .F.,
 ( 4, 4 ),
 ( 0.001875451646902783712, 0.003761979286331212577 ),
 .UNSPECIFIED. ) ;
#6194 = CARTESIAN_POINT ( 'NONE',  ( 34.00000000000000000, 28.19616000222403329, 4.163799117100999770E-15 ) ) ;
#6195 = CARTESIAN_POINT ( 'NONE',  ( -9.225358738174124440, 39.40776783337060607, 54.37884419088918975 ) ) ;
#6196 = DIRECTION ( 'NONE',  ( 0.000000000000000000, -0.7071067811865500152, -0.7071067811865451302 ) ) ;
#6197 = PRESENTATION_LAYER_ASSIGNMENT (  '', '', ( #8749 ) ) ;
#6198 = ORIENTED_EDGE ( 'NONE', *, *, #4183, .T. ) ;
#6199 = DIRECTION ( 'NONE',  ( 0.000000000000000000, 0.000000000000000000, 1.000000000000000000 ) ) ;
#6200 = CYLINDRICAL_SURFACE ( 'NONE', #19551, 10.00000000000000000 ) ;
#6201 = CARTESIAN_POINT ( 'NONE',  ( -0.03103604280932474244, 39.99999434194312897, -48.75811830434601291 ) ) ;
#6202 = ORIENTED_EDGE ( 'NONE', *, *, #17180, .T. ) ;
#6203 = ADVANCED_FACE ( 'NONE', ( #15502 ), #22646, .T. ) ;
#6204 = CARTESIAN_POINT ( 'NONE',  ( -15.00000000000001066, 20.77286304060557853, 45.82575694955839651 ) ) ;
#6205 = DIRECTION ( 'NONE',  ( -6.505213034913038160E-19, -3.903127820947822896E-18, -1.000000000000000000 ) ) ;
#6206 = PRODUCT_DEFINITION_SHAPE ( 'NONE', 'NONE',  #22702 ) ;
#6207 = EDGE_CURVE ( 'NONE', #8659, #3991, #3985, .T. ) ;
#6208 = VERTEX_POINT ( 'NONE', #46 ) ;
#6209 = VERTEX_POINT ( 'NONE', #13994 ) ;
#6210 = CARTESIAN_POINT ( 'NONE',  ( 118.4765993175494145, 176.9772506151337552, -48.50164097657800255 ) ) ;
#6211 = VERTEX_POINT ( 'NONE', #12305 ) ;
#6212 = CARTESIAN_POINT ( 'NONE',  ( 17.90966157241560452, 28.91510314404816384, -60.08313820791175885 ) ) ;
#6213 = ADVANCED_FACE ( 'NONE', ( #17576 ), #6634, .F. ) ;
#6214 = DIRECTION ( 'NONE',  ( 1.000000000000000000, 0.000000000000000000, 0.000000000000000000 ) ) ;
#6215 = DIRECTION ( 'NONE',  ( 1.000000000000000000, 0.000000000000000000, 0.000000000000000000 ) ) ;
#6216 = CARTESIAN_POINT ( 'NONE',  ( -34.99999999999999289, -5.000000000000000000, -57.00000000000000711 ) ) ;
#6217 = DIRECTION ( 'NONE',  ( 6.505213034913038160E-19, 3.903127820947822896E-18, 1.000000000000000000 ) ) ;
#6218 = ORIENTED_EDGE ( 'NONE', *, *, #9082, .F. ) ;
#6219 = CYLINDRICAL_SURFACE ( 'NONE', #11672, 6.499999999999999112 ) ;
#6220 = CARTESIAN_POINT ( 'NONE',  ( -37.07861450834799655, 3.656418565263969356, -7.000000000000006217 ) ) ;
#6221 = ORIENTED_EDGE ( 'NONE', *, *, #8412, .T. ) ;
#6222 = DIRECTION ( 'NONE',  ( -6.505213034913038160E-19, -3.903127820947822896E-18, -1.000000000000000000 ) ) ;
#6223 = CARTESIAN_POINT ( 'NONE',  ( -35.00000000000000000, 17.00000000000000000, 39.00000000000003553 ) ) ;
#6225 = AXIS2_PLACEMENT_3D ( 'NONE', #1390, #11805, #6775 ) ;
#6224 = DIRECTION ( 'NONE',  ( 8.659560562355114050E-17, 0.7071067811865326957, -0.7071067811865622277 ) ) ;
#6226 = CARTESIAN_POINT ( 'NONE',  ( 17.38307674301854533, 10.07685590252457253, -59.93367040492843500 ) ) ;
#6227 = ORIENTED_EDGE ( 'NONE', *, *, #10126, .F. ) ;
#6228 = FACE_OUTER_BOUND ( 'NONE', #16783, .T. ) ;
#6229 = CARTESIAN_POINT ( 'NONE',  ( 1.575045212608050749, 39.94053886632075745, -50.55745523153133547 ) ) ;
#6230 = ORIENTED_EDGE ( 'NONE', *, *, #11869, .F. ) ;
#6231 = CARTESIAN_POINT ( 'NONE',  ( 5.702716825708685100, 39.17357718829572377, 54.58701425222751169 ) ) ;
#6232 = CARTESIAN_POINT ( 'NONE',  ( 0.2893518482366595479, -0.01224439107861633597, -48.63017502620383681 ) ) ;
#6233 = VERTEX_POINT ( 'NONE', #3947 ) ;
#6234 = PRODUCT_DEFINITION_CONTEXT ( 'detailed design', #7112, 'design' ) ;
#6235 = EDGE_CURVE ( 'NONE', #3953, #14343, #7717, .T. ) ;
#6236 = CIRCLE ( 'NONE', #10239, 2.525000000000110489 ) ;
#6237 = CARTESIAN_POINT ( 'NONE',  ( 11.24237306623960819, 36.54654314592769282, 57.72256821685510175 ) ) ;
#6238 = DIRECTION ( 'NONE',  ( 1.000000000000000000, 1.208970125616062874E-17, 0.000000000000000000 ) ) ;
#6239 = CARTESIAN_POINT ( 'NONE',  ( 19.66964734151795113, 9.174855960407793276, -58.00890637771954772 ) ) ;
#6240 = EDGE_CURVE ( 'NONE', #15452, #17708, #21350, .T. ) ;
#6241 = ORIENTED_EDGE ( 'NONE', *, *, #8304, .T. ) ;
#6242 = AXIS2_PLACEMENT_3D ( 'NONE', #318, #195, #7191 ) ;
#6243 = EDGE_LOOP ( 'NONE', ( #16437, #8303, #5852, #1716 ) ) ;
#6244 = ORIENTED_EDGE ( 'NONE', *, *, #14854, .F. ) ;
#6245 = EDGE_LOOP ( 'NONE', ( #4620, #15567, #19165, #4649 ) ) ;
#6246 = CARTESIAN_POINT ( 'NONE',  ( 2.916776610577574314, 22.79308088018310841, 6.515718972866975989 ) ) ;
#6247 = LINE ( 'NONE', #13206, #2611 ) ;
#6248 = ADVANCED_FACE ( 'NONE', ( #2103 ), #16787, .F. ) ;
#6249 = VERTEX_POINT ( 'NONE', #21590 ) ;
#6250 = DIRECTION ( 'NONE',  ( -1.000000000000000000, 1.264902534566437206E-16, 0.000000000000000000 ) ) ;
#6251 = CARTESIAN_POINT ( 'NONE',  ( 2.615700731154975145, 14.48345912138648295, 6.612978332551282534 ) ) ;
#6252 = ORIENTED_EDGE ( 'NONE', *, *, #22220, .F. ) ;
#6253 = CARTESIAN_POINT ( 'NONE',  ( 35.00000000000000000, 10.00000000000000000, -40.99999999999997868 ) ) ;
#6254 = ORIENTED_EDGE ( 'NONE', *, *, #8021, .F. ) ;
#6255 = FACE_OUTER_BOUND ( 'NONE', #20097, .T. ) ;
#6256 = EDGE_CURVE ( 'NONE', #5255, #14343, #10170, .T. ) ;
#6257 = DIRECTION ( 'NONE',  ( 1.049727191138618326E-16, -0.5150380749100547106, 0.8571673007021120005 ) ) ;
#6258 = DIRECTION ( 'NONE',  ( -1.000000000000000000, -1.208970125616081209E-17, 0.000000000000000000 ) ) ;
#6259 = CARTESIAN_POINT ( 'NONE',  ( -0.2369887982023440309, 39.99966998679947494, 48.91756878588413571 ) ) ;
#6260 = VECTOR ( 'NONE', #11248, 1000.000000000000000 ) ;
#6261 = EDGE_CURVE ( 'NONE', #15308, #12719, #8354, .T. ) ;
#6262 = CARTESIAN_POINT ( 'NONE',  ( -14.17374118098246605, 15.07546459525164728, 45.45638825402603089 ) ) ;
#6263 = CARTESIAN_POINT ( 'NONE',  ( -16.06969024216331476, -19.15111107797465451, 2.999999999999995559 ) ) ;
#6264 = ORIENTED_EDGE ( 'NONE', *, *, #21917, .T. ) ;
#6265 = ORIENTED_EDGE ( 'NONE', *, *, #12250, .F. ) ;
#6266 = EDGE_CURVE ( 'NONE', #9062, #16838, #14181, .T. ) ;
#6267 = ORIENTED_EDGE ( 'NONE', *, *, #12925, .T. ) ;
#6268 = CARTESIAN_POINT ( 'NONE',  ( -19.98434069128082058, 21.18673122687496502, 60.61816909402018183 ) ) ;
#6269 = CARTESIAN_POINT ( 'NONE',  ( 29.33526866242108611, -22.15900668633799597, -1.999999999999980904 ) ) ;
#6270 = VECTOR ( 'NONE', #10305, 1000.000000000000000 ) ;
#6271 = EDGE_CURVE ( 'NONE', #22398, #8190, #14582, .T. ) ;
#6272 = DIRECTION ( 'NONE',  ( 0.000000000000000000, 0.000000000000000000, -1.000000000000000000 ) ) ;
#6273 = FACE_OUTER_BOUND ( 'NONE', #6832, .T. ) ;
#6274 = EDGE_CURVE ( 'NONE', #3399, #18007, #2455, .T. ) ;
#6275 = DIRECTION ( 'NONE',  ( -1.000000000000000000, -4.175647542716197082E-14, 0.000000000000000000 ) ) ;
#6276 = CARTESIAN_POINT ( 'NONE',  ( 5.666159602074075430, 39.18446031140960883, 54.55708815122284250 ) ) ;
#6277 = CARTESIAN_POINT ( 'NONE',  ( -2.881553265153760979, 39.80724590269267082, -51.34430246875412962 ) ) ;
#6278 = DIRECTION ( 'NONE',  ( 0.000000000000000000, 1.000000000000000000, 0.000000000000000000 ) ) ;
#6279 = VECTOR ( 'NONE', #17667, 1000.000000000000000 ) ;
#6280 = AXIS2_PLACEMENT_3D ( 'NONE', #7933, #15119, #18587 ) ;
#6281 = ORIENTED_EDGE ( 'NONE', *, *, #3401, .T. ) ;
#6282 = CARTESIAN_POINT ( 'NONE',  ( -11.17438353593063560, 39.11312751358374840, 55.08132213033135116 ) ) ;
#6283 = DIRECTION ( 'NONE',  ( 0.000000000000000000, 0.000000000000000000, -1.000000000000000000 ) ) ;
#6284 = DIRECTION ( 'NONE',  ( -6.505213034913038160E-19, -3.903127820947822896E-18, -1.000000000000000000 ) ) ;
#6285 = ORIENTED_EDGE ( 'NONE', *, *, #21853, .T. ) ;
#6286 = DIRECTION ( 'NONE',  ( -6.505213034913038160E-19, -3.903127820947822896E-18, -1.000000000000000000 ) ) ;
#6287 = DIRECTION ( 'NONE',  ( -1.000000000000000000, -1.208970125616044077E-17, 0.000000000000000000 ) ) ;
#6288 = DIRECTION ( 'NONE',  ( 1.000000000000000000, 0.000000000000000000, 0.000000000000000000 ) ) ;
#6289 = EDGE_CURVE ( 'NONE', #8848, #349, #20074, .T. ) ;
#6290 = DIRECTION ( 'NONE',  ( -0.000000000000000000, -0.000000000000000000, -1.000000000000000000 ) ) ;
#6291 = VECTOR ( 'NONE', #10886, 1000.000000000000000 ) ;
#6292 = CARTESIAN_POINT ( 'NONE',  ( 6.094655612023198721, 39.99999999999999289, -52.13899149650791998 ) ) ;
#6293 = EDGE_LOOP ( 'NONE', ( #10660, #3420 ) ) ;
#6294 = CARTESIAN_POINT ( 'NONE',  ( 4.591787867733965633, 39.86870494181058433, -51.95898231442010484 ) ) ;
#6295 = DIRECTION ( 'NONE',  ( 0.000000000000000000, 0.000000000000000000, 1.000000000000000000 ) ) ;
#6296 = ADVANCED_FACE ( 'NONE', ( #11260 ), #13101, .T. ) ;
#6297 = DIRECTION ( 'NONE',  ( 0.000000000000000000, 1.000000000000000000, 0.000000000000000000 ) ) ;
#6298 = DIRECTION ( 'NONE',  ( -1.067522139062650671E-15, 0.000000000000000000, -1.000000000000000000 ) ) ;
#6299 = CARTESIAN_POINT ( 'NONE',  ( -34.99999999999999289, 0.000000000000000000, -3.012171160963566127E-14 ) ) ;
#6300 = CARTESIAN_POINT ( 'NONE',  ( -6.215602297253691511, 39.75345783577535741, 52.92318667896167739 ) ) ;
#6301 = CARTESIAN_POINT ( 'NONE',  ( 13.33780792070359666, 2.142135623730922589, -45.06383732350882809 ) ) ;
#6302 = VERTEX_POINT ( 'NONE', #14458 ) ;
#6303 = DIRECTION ( 'NONE',  ( -6.505213034913038160E-19, -3.903127820947822896E-18, -1.000000000000000000 ) ) ;
#6304 = DIRECTION ( 'NONE',  ( 1.000000000000000000, 0.000000000000000000, 0.000000000000000000 ) ) ;
#6305 = CARTESIAN_POINT ( 'NONE',  ( -29.33526866242079478, 22.15900668633771886, 2.800654218530485018 ) ) ;
#6306 = EDGE_CURVE ( 'NONE', #15747, #7646, #16027, .T. ) ;
#6307 = ORIENTED_EDGE ( 'NONE', *, *, #4969, .T. ) ;
#6308 = CIRCLE ( 'NONE', #1186, 4.000000000000000000 ) ;
#6309 = DIRECTION ( 'NONE',  ( 0.000000000000000000, 0.000000000000000000, -1.000000000000000000 ) ) ;
#6310 = FACE_OUTER_BOUND ( 'NONE', #7965, .T. ) ;
#6311 = ADVANCED_FACE ( 'NONE', ( #5887 ), #21815, .T. ) ;
#6312 = ORIENTED_EDGE ( 'NONE', *, *, #10579, .F. ) ;
#6313 = ORIENTED_EDGE ( 'NONE', *, *, #21498, .F. ) ;
#6314 = DIRECTION ( 'NONE',  ( -0.9369493372187405189, -0.3494420069955173069, -0.004027807382165029225 ) ) ;
#6315 = VERTEX_POINT ( 'NONE', #9323 ) ;
#6316 = CARTESIAN_POINT ( 'NONE',  ( 16.96028156848954183, 30.61033039275981338, -59.80781543853671423 ) ) ;
#6317 = DIRECTION ( 'NONE',  ( -3.525918314278899701E-15, 0.000000000000000000, 1.000000000000000000 ) ) ;
#6318 = CIRCLE ( 'NONE', #19136, 2.500000000000002220 ) ;
#6319 = AXIS2_PLACEMENT_3D ( 'NONE', #13885, #20902, #8299 ) ;
#6320 = DIRECTION ( 'NONE',  ( -0.000000000000000000, 1.000000000000000000, -0.000000000000000000 ) ) ;
#6321 = CARTESIAN_POINT ( 'NONE',  ( -10.34893680499411239, 34.64233806479123956, 2.932969818539072016 ) ) ;
#6322 = FACE_OUTER_BOUND ( 'NONE', #10656, .T. ) ;
#6323 = VERTEX_POINT ( 'NONE', #4170 ) ;
#6324 = CARTESIAN_POINT ( 'NONE',  ( -14.67611967928904271, 31.67162468655987340, 3.000000000000009770 ) ) ;
#6325 = DIRECTION ( 'NONE',  ( -0.000000000000000000, -1.000000000000000000, -0.000000000000000000 ) ) ;
#6326 = ORIENTED_EDGE ( 'NONE', *, *, #5832, .T. ) ;
#6327 = CARTESIAN_POINT ( 'NONE',  ( -13.75658951623324455, 14.00814961052207686, -45.26303799332215050 ) ) ;
#6328 = CONICAL_SURFACE ( 'NONE', #12897, 2.524999999999999467, 0.7853981633974482790 ) ;
#6329 = DIRECTION ( 'NONE',  ( -0.000000000000000000, 1.000000000000000000, -0.000000000000000000 ) ) ;
#6330 = LINE ( 'NONE', #13289, #10426 ) ;
#6331 = CARTESIAN_POINT ( 'NONE',  ( -15.50000000000011013, 42.51666049839536043, 60.00099999999999767 ) ) ;
#6332 = VERTEX_POINT ( 'NONE', #12854 ) ;
#6333 = DIRECTION ( 'NONE',  ( -0.000000000000000000, 1.000000000000000000, 0.000000000000000000 ) ) ;
#6334 = CARTESIAN_POINT ( 'NONE',  ( 6.775203351379166961, 38.82189279864962828, -55.41163305959238983 ) ) ;
#6335 = ORIENTED_EDGE ( 'NONE', *, *, #4640, .T. ) ;
#6336 = DIRECTION ( 'NONE',  ( 1.000000000000000000, 1.208970125616063490E-17, 0.000000000000000000 ) ) ;
#6337 = EDGE_CURVE ( 'NONE', #17762, #15630, #2792, .T. ) ;
#6338 = CARTESIAN_POINT ( 'NONE',  ( -7.577104390338837980, -0.4826542685308990444, 53.01683071947941528 ) ) ;
#6339 = EDGE_LOOP ( 'NONE', ( #20543, #3126, #6966, #9548, #10328, #5530 ) ) ;
#6340 = CARTESIAN_POINT ( 'NONE',  ( 10.55176496409977283, 37.02956028564562985, 54.80914071361393525 ) ) ;
#6341 = DIRECTION ( 'NONE',  ( -0.000000000000000000, 1.000000000000000000, -0.000000000000000000 ) ) ;
#6342 = ADVANCED_FACE ( 'NONE', ( #11606 ), #9887, .T. ) ;
#6343 = VECTOR ( 'NONE', #8104, 1000.000000000000000 ) ;
#6344 = CARTESIAN_POINT ( 'NONE',  ( 20.01613897800084985, 20.29830884309071948, -58.15166638930550391 ) ) ;
#6345 = CIRCLE ( 'NONE', #17308, 20.00000000000000000 ) ;
#6346 = ORIENTED_EDGE ( 'NONE', *, *, #8898, .F. ) ;
#6347 = ORIENTED_EDGE ( 'NONE', *, *, #20668, .F. ) ;
#6348 = ORIENTED_EDGE ( 'NONE', *, *, #3893, .F. ) ;
#6349 = ORIENTED_EDGE ( 'NONE', *, *, #3101, .F. ) ;
#6350 = CARTESIAN_POINT ( 'NONE',  ( 10.44987231559219509, 39.22455541040593374, 54.81340832989639722 ) ) ;
#6351 = FACE_OUTER_BOUND ( 'NONE', #11182, .T. ) ;
#6352 = EDGE_CURVE ( 'NONE', #19351, #3791, #12570, .T. ) ;
#6353 = ORIENTED_EDGE ( 'NONE', *, *, #15331, .T. ) ;
#6354 = CARTESIAN_POINT ( 'NONE',  ( -42.50000000000000711, -5.000000000000000000, -47.50000000000000000 ) ) ;
#6355 = DIRECTION ( 'NONE',  ( 0.000000000000000000, 0.000000000000000000, 1.000000000000000000 ) ) ;
#6356 = EDGE_LOOP ( 'NONE', ( #17357, #7718 ) ) ;
#6357 = DIRECTION ( 'NONE',  ( 6.505213034913038160E-19, 3.903127820947822896E-18, 1.000000000000000000 ) ) ;
#6358 = CARTESIAN_POINT ( 'NONE',  ( 10.60627602730290242, 0.5940385038070811197, 54.69850067894081036 ) ) ;
#6359 = VECTOR ( 'NONE', #9597, 1000.000000000000000 ) ;
#6360 = VERTEX_POINT ( 'NONE', #11493 ) ;
#6361 = CARTESIAN_POINT ( 'NONE',  ( -1.128083539116253586, -34.88850421923977763, -2.999999999999971578 ) ) ;
#6362 = CIRCLE ( 'NONE', #19173, 2.500000000000002220 ) ;
#6363 = CARTESIAN_POINT ( 'NONE',  ( 2.220446049250313081E-13, -2.498001805406602216E-13, -6.859353255829918616 ) ) ;
#6364 = ADVANCED_FACE ( 'NONE', ( #20207 ), #4628, .F. ) ;
#6365 = LINE ( 'NONE', #642, #21071 ) ;
#6366 = EDGE_CURVE ( 'NONE', #18860, #6323, #16417, .T. ) ;
#6367 = FACE_OUTER_BOUND ( 'NONE', #3757, .T. ) ;
#6368 = CIRCLE ( 'NONE', #2713, 2.500000000000002220 ) ;
#6369 = CONICAL_SURFACE ( 'NONE', #4901, 17.00000000000001421, 0.7853981633974603804 ) ;
#6370 = DIRECTION ( 'NONE',  ( -1.000000000000000000, 0.000000000000000000, 0.000000000000000000 ) ) ;
#6371 = EDGE_LOOP ( 'NONE', ( #10254, #12126, #33, #7562 ) ) ;
#6372 = ORIENTED_EDGE ( 'NONE', *, *, #22158, .F. ) ;
#6373 = VECTOR ( 'NONE', #811, 1000.000000000000000 ) ;
#6374 = ORIENTED_EDGE ( 'NONE', *, *, #19658, .F. ) ;
#6375 = CARTESIAN_POINT ( 'NONE',  ( -19.66964734151719085, 9.174855960407388267, 58.00890637771936298 ) ) ;
#6376 = CARTESIAN_POINT ( 'NONE',  ( 6.123233995736766282E-16, -45.00000000000000000, -5.000000000000000000 ) ) ;
#6377 = EDGE_CURVE ( 'NONE', #19404, #6211, #687, .T. ) ;
#6378 = CARTESIAN_POINT ( 'NONE',  ( -11.68090480754633731, 3.765577839755393619, -57.90797000640141334 ) ) ;
#6379 = DIRECTION ( 'NONE',  ( 0.000000000000000000, 0.000000000000000000, -1.000000000000000000 ) ) ;
#6380 = DIRECTION ( 'NONE',  ( 0.000000000000000000, 0.000000000000000000, 1.000000000000000000 ) ) ;
#6381 = ORIENTED_EDGE ( 'NONE', *, *, #15884, .F. ) ;
#6382 = VECTOR ( 'NONE', #9045, 1000.000000000000000 ) ;
#6383 = CARTESIAN_POINT ( 'NONE',  ( -23.50000000000001066, 19.99999999999982947, -100.0000000000000000 ) ) ;
#6384 = CARTESIAN_POINT ( 'NONE',  ( 29.14949368109878591, -11.93972437435561496, 3.000000000000023537 ) ) ;
#6385 = CARTESIAN_POINT ( 'NONE',  ( -9.999999999999998224, 12.49999999999999645, 3.000000000000000000 ) ) ;
#6386 = ADVANCED_FACE ( 'NONE', ( #19930 ), #21419, .F. ) ;
#6387 = CARTESIAN_POINT ( 'NONE',  ( 9.377138775072179300, -4.928932188134423242, 51.00555535510625305 ) ) ;
#6388 = EDGE_CURVE ( 'NONE', #10638, #9680, #1970, .T. ) ;
#6389 = DIRECTION ( 'NONE',  ( 0.000000000000000000, 0.000000000000000000, 1.000000000000000000 ) ) ;
#6390 = EDGE_CURVE ( 'NONE', #6724, #18961, #8207, .T. ) ;
#6391 = EDGE_LOOP ( 'NONE', ( #13678, #4858, #16982, #3070 ) ) ;
#6392 = DIRECTION ( 'NONE',  ( -6.505213034913038160E-19, -3.903127820947822896E-18, -1.000000000000000000 ) ) ;
#6393 = DIRECTION ( 'NONE',  ( 1.000000000000000000, 0.000000000000000000, 0.000000000000000000 ) ) ;
#6394 = CIRCLE ( 'NONE', #14373, 2.500000000000002220 ) ;
#6395 = EDGE_CURVE ( 'NONE', #19660, #16550, #11212, .T. ) ;
#6396 = ORIENTED_EDGE ( 'NONE', *, *, #3868, .F. ) ;
#6397 = DIRECTION ( 'NONE',  ( 1.000000000000000000, 0.000000000000000000, 0.000000000000000000 ) ) ;
#6398 = FACE_OUTER_BOUND ( 'NONE', #16860, .T. ) ;
#6399 = CARTESIAN_POINT ( 'NONE',  ( 0.000000000000000000, 15.00000000000000000, 3.399999999999995470 ) ) ;
#6400 = EDGE_CURVE ( 'NONE', #6131, #2785, #12068, .T. ) ;
#6401 = ORIENTED_EDGE ( 'NONE', *, *, #6908, .F. ) ;
#6402 = CLOSED_SHELL ( 'NONE', ( #11558, #15977, #21072, #17552, #10476, #3164, #18971, #1160, #7877, #11153, #8622, #6184, #18030, #15032, #8107, #18639, #7981, #8561, #12450, #1201, #21163, #4682, #15367, #6342, #11464, #17295, #3419, #277, #20808, #14905, #17848, #17728, #14298, #21900, #7231, #8117, #3944, #805, #17868, #8429, #10529, #8480, #10844, #18939, #1902, #9631, #14345, #2341, #19798 ) ) ;
#6403 = VERTEX_POINT ( 'NONE', #445 ) ;
#6404 = CIRCLE ( 'NONE', #7120, 5.000000000000000000 ) ;
#6405 = CARTESIAN_POINT ( 'NONE',  ( -10.27431133777638550, -4.928932188134511172, 51.43682631505698311 ) ) ;
#6406 = CARTESIAN_POINT ( 'NONE',  ( -25.00000000000000000, 20.00000000000000000, -25.00000000000000000 ) ) ;
#6407 = ORIENTED_EDGE ( 'NONE', *, *, #5547, .T. ) ;
#6408 = CYLINDRICAL_SURFACE ( 'NONE', #15744, 2.500000000000002220 ) ;
#6409 = CARTESIAN_POINT ( 'NONE',  ( 28.96193690644957641, 14.74639653023213093, -6.999999999999950262 ) ) ;
#6410 = FACE_OUTER_BOUND ( 'NONE', #8750, .T. ) ;
#6411 = CIRCLE ( 'NONE', #8953, 34.90673715956759082 ) ;
#6412 = CARTESIAN_POINT ( 'NONE',  ( -13.06496334682255167, 4.761428254742599897, -58.49034434778481994 ) ) ;
#6413 = CARTESIAN_POINT ( 'NONE',  ( -10.63866000424708602, 30.58060543830995570, -43.66469350997155630 ) ) ;
#6414 = AXIS2_PLACEMENT_3D ( 'NONE', #700, #20062, #2534 ) ;
#6415 = CARTESIAN_POINT ( 'NONE',  ( 13.00000000000000178, 20.00000000000000000, -11.32475165290605723 ) ) ;
#6416 = VERTEX_POINT ( 'NONE', #5948 ) ;
#6417 = CYLINDRICAL_SURFACE ( 'NONE', #5367, 2.099999999999997868 ) ;
#6418 = DIRECTION ( 'NONE',  ( -6.505213034913038160E-19, -3.903127820947822896E-18, -1.000000000000000000 ) ) ;
#6419 = DIRECTION ( 'NONE',  ( 0.000000000000000000, 1.000000000000000000, 0.000000000000000000 ) ) ;
#6420 = DIRECTION ( 'NONE',  ( 1.000000000000000000, 0.000000000000000000, 0.000000000000000000 ) ) ;
#6421 = EDGE_CURVE ( 'NONE', #691, #6233, #22465, .T. ) ;
#6422 = ORIENTED_EDGE ( 'NONE', *, *, #6998, .F. ) ;
#6423 = ADVANCED_FACE ( 'NONE', ( #14645 ), #796, .F. ) ;
#6424 = CARTESIAN_POINT ( 'NONE',  ( -2.422192751863727622, -32.40961249803553557, -6.999999999999950262 ) ) ;
#6425 = DIRECTION ( 'NONE',  ( -1.000000000000000000, 0.000000000000000000, 0.000000000000000000 ) ) ;
#6426 = ADVANCED_FACE ( 'NONE', ( #12809 ), #14530, .T. ) ;
#6427 = AXIS2_PLACEMENT_3D ( 'NONE', #4637, #13420, #22622 ) ;
#6428 = VERTEX_POINT ( 'NONE', #19821 ) ;
#6429 = TOROIDAL_SURFACE ( 'NONE', #5339, 34.90673715956759082, 8.750000000000000000 ) ;
#6430 = AXIS2_PLACEMENT_3D ( 'NONE', #22070, #14826, #20236 ) ;
#6431 = ORIENTED_EDGE ( 'NONE', *, *, #18017, .T. ) ;
#6432 = VECTOR ( 'NONE', #6881, 1000.000000000000000 ) ;
#6433 = CONTEXT_DEPENDENT_SHAPE_REPRESENTATION ( #8727, #13315 ) ;
#6434 = ORIENTED_EDGE ( 'NONE', *, *, #13250, .T. ) ;
#6435 = CARTESIAN_POINT ( 'NONE',  ( 9.958219108218454352, 37.43657071496331668, -57.18097912447547060 ) ) ;
#6436 = CARTESIAN_POINT ( 'NONE',  ( -25.00000000000000000, 20.00000000000000000, -16.49999999999998934 ) ) ;
#6437 = DIRECTION ( 'NONE',  ( -0.000000000000000000, -0.000000000000000000, 1.000000000000000000 ) ) ;
#6438 = CARTESIAN_POINT ( 'NONE',  ( 7.310544252644470693E-15, 28.19616000222403684, 0.000000000000000000 ) ) ;
#6439 = CARTESIAN_POINT ( 'NONE',  ( -42.50000000000000711, -12.00000000000000000, -45.40000000000000568 ) ) ;
#6440 = ORIENTED_EDGE ( 'NONE', *, *, #8868, .T. ) ;
#6441 = CARTESIAN_POINT ( 'NONE',  ( -35.00000000000000000, 40.00000000000000000, -59.99999999999998579 ) ) ;
#6442 = CARTESIAN_POINT ( 'NONE',  ( 17.99999999999998579, 20.00000000000000355, 103.0000000000000284 ) ) ;
#6443 = EDGE_LOOP ( 'NONE', ( #14324, #4513, #18662, #19273 ) ) ;
#6444 = CARTESIAN_POINT ( 'NONE',  ( -11.37797799463865722, 10.21854205506534008, -44.06891764425669322 ) ) ;
#6445 = CYLINDRICAL_SURFACE ( 'NONE', #9750, 19.11328065563151668 ) ;
#6446 = EDGE_CURVE ( 'NONE', #6315, #8022, #3811, .T. ) ;
#6447 = DIRECTION ( 'NONE',  ( 0.000000000000000000, 0.000000000000000000, 1.000000000000000000 ) ) ;
#6448 = CARTESIAN_POINT ( 'NONE',  ( -36.75746821813285692, 0.6841746959066752343, -2.800654218530457484 ) ) ;
#6449 = ORIENTED_EDGE ( 'NONE', *, *, #14981, .T. ) ;
#6450 = DIRECTION ( 'NONE',  ( 0.000000000000000000, 0.000000000000000000, 1.000000000000000000 ) ) ;
#6451 = ORIENTED_EDGE ( 'NONE', *, *, #16328, .T. ) ;
#6452 = CARTESIAN_POINT ( 'NONE',  ( 6.261274683082145742, 0.9579800028911629184, -54.84444022978222932 ) ) ;
#6453 = AXIS2_PLACEMENT_3D ( 'NONE', #11601, #8391, #4844 ) ;
#6454 = AXIS2_PLACEMENT_3D ( 'NONE', #1222, #9930, #22550 ) ;
#6455 = CIRCLE ( 'NONE', #11584, 34.00000000000000000 ) ;
#6456 = AXIS2_PLACEMENT_3D ( 'NONE', #22586, #13843, #14172 ) ;
#6457 = ORIENTED_EDGE ( 'NONE', *, *, #9839, .T. ) ;
#6458 = FACE_OUTER_BOUND ( 'NONE', #7366, .T. ) ;
#6459 = FACE_OUTER_BOUND ( 'NONE', #9454, .T. ) ;
#6460 = FACE_OUTER_BOUND ( 'NONE', #11533, .T. ) ;
#6461 = AXIS2_PLACEMENT_3D ( 'NONE', #5493, #440, #19818 ) ;
#6462 = CARTESIAN_POINT ( 'NONE',  ( 19.66835476179213416, 23.72826198822077615, -58.05955247658420149 ) ) ;
#6463 = EDGE_LOOP ( 'NONE', ( #747, #17147, #21994, #860 ) ) ;
#6464 = VERTEX_POINT ( 'NONE', #13147 ) ;
#6465 = ORIENTED_EDGE ( 'NONE', *, *, #8090, .F. ) ;
#6466 = AXIS2_PLACEMENT_3D ( 'NONE', #2222, #16182, #492 ) ;
#6467 = EDGE_CURVE ( 'NONE', #17839, #9501, #4467, .T. ) ;
#6468 = VERTEX_POINT ( 'NONE', #11445 ) ;
#6469 = CARTESIAN_POINT ( 'NONE',  ( 0.1993075993174698302, 24.99978691316126955, 6.999930029250658770 ) ) ;
#6470 = VERTEX_POINT ( 'NONE', #2747 ) ;
#6471 = DIRECTION ( 'NONE',  ( -0.000000000000000000, -1.000000000000000000, -0.000000000000000000 ) ) ;
#6472 = CARTESIAN_POINT ( 'NONE',  ( -10.27431133777642458, -4.928932188134513837, -51.43682631505698311 ) ) ;
#6473 = ORIENTED_EDGE ( 'NONE', *, *, #15600, .F. ) ;
#6474 = CARTESIAN_POINT ( 'NONE',  ( -10.00000000000000888, 3.000000000000002665, 5.000000000000000888 ) ) ;
#6475 = EDGE_CURVE ( 'NONE', #1368, #8806, #7438, .T. ) ;
#6476 = AXIS2_PLACEMENT_3D ( 'NONE', #2717, #7863, #4096 ) ;
#6477 = EDGE_LOOP ( 'NONE', ( #18131, #3618, #5208, #606 ) ) ;
#6478 = FACE_OUTER_BOUND ( 'NONE', #20915, .T. ) ;
#6479 = DIRECTION ( 'NONE',  ( -6.505213034913038160E-19, -3.903127820947822896E-18, -1.000000000000000000 ) ) ;
#6480 = DIRECTION ( 'NONE',  ( -1.000000000000000000, 0.000000000000000000, 0.000000000000000000 ) ) ;
#6481 = DIRECTION ( 'NONE',  ( -1.000000000000000000, -1.208970125616060101E-17, 6.505213034913038160E-19 ) ) ;
#6482 = CIRCLE ( 'NONE', #22243, 2.500000000000002220 ) ;
#6483 = DIRECTION ( 'NONE',  ( -0.000000000000000000, -0.000000000000000000, -1.000000000000000000 ) ) ;
#6484 = EDGE_CURVE ( 'NONE', #9968, #17215, #686, .T. ) ;
#6485 = ORIENTED_EDGE ( 'NONE', *, *, #15815, .T. ) ;
#6486 = ORIENTED_EDGE ( 'NONE', *, *, #12226, .F. ) ;
#6487 = EDGE_CURVE ( 'NONE', #2718, #19753, #19719, .T. ) ;
#6488 = ORIENTED_EDGE ( 'NONE', *, *, #10845, .F. ) ;
#6489 = CARTESIAN_POINT ( 'NONE',  ( -16.98435752850986091, 5.286895767878122321, 57.23469700293563278 ) ) ;
#6490 = CARTESIAN_POINT ( 'NONE',  ( 16.56444186175090749, -26.79308242454900224, -7.000000000000006217 ) ) ;
#6491 = CIRCLE ( 'NONE', #1732, 2.099999999999997868 ) ;
#6492 = TOROIDAL_SURFACE ( 'NONE', #15238, 34.90673715956759082, 8.750000000000000000 ) ;
#6493 = CARTESIAN_POINT ( 'NONE',  ( -20.00000000000002487, 18.38876824873586457, -60.62177826491085142 ) ) ;
#6494 = CARTESIAN_POINT ( 'NONE',  ( 28.52469787935785561, 7.000000000000000000, 4.095854054471903538 ) ) ;
#6495 = CIRCLE ( 'NONE', #18569, 1.000000000000000888 ) ;
#6496 = DIRECTION ( 'NONE',  ( 6.505213034913038160E-19, 3.903127820947822896E-18, 1.000000000000000000 ) ) ;
#6497 = EDGE_LOOP ( 'NONE', ( #18272, #14911, #16477, #5249 ) ) ;
#6498 = DIRECTION ( 'NONE',  ( 0.000000000000000000, -1.000000000000000000, 0.000000000000000000 ) ) ;
#6499 = CARTESIAN_POINT ( 'NONE',  ( -4.769735313644264174, 39.99999999999999289, -51.49386057199703970 ) ) ;
#6500 = DIRECTION ( 'NONE',  ( 0.000000000000000000, 0.000000000000000000, 1.000000000000000000 ) ) ;
#6501 = DIRECTION ( 'NONE',  ( 6.505213034913038160E-19, 3.903127820947822896E-18, 1.000000000000000000 ) ) ;
#6502 = SHAPE_REPRESENTATION ( 'BOLT', ( #18273 ), #20471 ) ;
#6503 = ORIENTED_EDGE ( 'NONE', *, *, #20630, .T. ) ;
#6504 = AXIS2_PLACEMENT_3D ( 'NONE', #11704, #9973, #4498 ) ;
#6505 = CIRCLE ( 'NONE', #15272, 57.00000000000002132 ) ;
#6506 = CARTESIAN_POINT ( 'NONE',  ( 19.99999999999999645, 4.500000000000004441, 3.306546357697853339E-15 ) ) ;
#6507 = CYLINDRICAL_SURFACE ( 'NONE', #4939, 31.50000000000001421 ) ;
#6508 = VERTEX_POINT ( 'NONE', #9272 ) ;
#6509 = CIRCLE ( 'NONE', #4687, 2.500000000000002220 ) ;
#6510 = DIRECTION ( 'NONE',  ( -0.000000000000000000, 1.000000000000000000, -0.000000000000000000 ) ) ;
#6511 = EDGE_CURVE ( 'NONE', #17407, #15147, #16255, .T. ) ;
#6512 = CARTESIAN_POINT ( 'NONE',  ( 47.83731665821556334, 10.00000000000000000, -38.93845529828706020 ) ) ;
#6513 = AXIS2_PLACEMENT_3D ( 'NONE', #1688, #11996, #5135 ) ;
#6514 = DIRECTION ( 'NONE',  ( 0.000000000000000000, 0.000000000000000000, -1.000000000000000000 ) ) ;
#6515 = AXIS2_PLACEMENT_3D ( 'NONE', #21399, #14159, #14272 ) ;
#6516 = ORIENTED_EDGE ( 'NONE', *, *, #8390, .T. ) ;
#6517 = ADVANCED_FACE ( 'NONE', ( #20277 ), #6018, .F. ) ;
#6518 = ADVANCED_FACE ( 'NONE', ( #11674 ), #22317, .T. ) ;
#6519 = EDGE_CURVE ( 'NONE', #9264, #15847, #13484, .T. ) ;
#6520 = ORIENTED_EDGE ( 'NONE', *, *, #1714, .F. ) ;
#6521 = CYLINDRICAL_SURFACE ( 'NONE', #16984, 36.76383501243555685 ) ;
#6522 = DIRECTION ( 'NONE',  ( 0.000000000000000000, 0.000000000000000000, -1.000000000000000000 ) ) ;
#6523 = EDGE_LOOP ( 'NONE', ( #4100, #13192, #20535, #17542 ) ) ;
#6524 = CONICAL_SURFACE ( 'NONE', #19343, 15.99999999999993072, 0.7853981633974415066 ) ;
#6525 = CYLINDRICAL_SURFACE ( 'NONE', #1116, 31.50000000000000711 ) ;
#6526 = B_SPLINE_CURVE_WITH_KNOTS ( 'NONE', 3,
 ( #8440, #1217, #8326, #22201, #15408, #6721, #15300, #19550, #5130, #15522, #15642, #19215, #1904, #20823, #8548, #13916, #22546, #17706, #8884, #14254, #14018, #6841, #13806, #293, #12102, #3640, #8786, #65, #8665, #7289, #21042, #10367, #21266, #5347, #19097, #17598, #5557, #21154, #3522, #3405, #12322, #168, #15981, #17363, #1683, #19333, #1561, #12536, #10594, #3853, #17251, #12430, #10700, #15858, #22671, #6958, #20933, #5232, #10483, #7166, #12213, #17482, #1801, #2012, #5458, #14135, #9000, #15755, #7055, #19442, #3745, #11288, #9570, #12876 ),
 .UNSPECIFIED., .F., .F.,
 ( 4, 2, 1, 2, 2, 1, 1, 2, 2, 2, 2, 1, 1, 1, 1, 1, 2, 2, 2, 1, 1, 1, 1, 1, 2, 2, 1, 1, 1, 1, 2, 2, 1, 1, 2, 2, 1, 2, 2, 2, 2, 1, 1, 2, 2, 2, 2, 4 ),
 ( 0.000000000000000000, 0.2499923706054147932, 0.2812414169310917256, 0.2851475477218011756, 0.2871006131171558451, 0.2890536785125104591, 0.2968659400939309134, 0.3124904632567707674, 0.3749885559081321817, 0.4999847412108561207, 0.5019378066062117894, 0.5038908720015674580, 0.5077970027922775742, 0.5156092643736978065, 0.5312337875365372719, 0.5624828338622163137, 0.6249809265135745084, 0.7499771118162896766, 0.7519301772116454563, 0.7538832426070012360, 0.7577893733977127955, 0.7656016349791360254, 0.7812261581419835954, 0.8124752044676776253, 0.8749732971190646857, 0.8769263625144214647, 0.8788794279097782436, 0.8827855587004908022, 0.8905978202819156975, 0.9062223434447642667, 0.9374713897704604060, 0.9413775205611728536, 0.9452836513518851902, 0.9530959129333099744, 0.9687204360961596539, 0.9726265668868717684, 0.9765326976775839940, 0.9843449592590070019, 0.9882510900497186723, 0.9921572208404302318, 0.9926454871892690379, 0.9931337535381078441, 0.9941102862357854564, 0.9960633516311395708, 0.9970398843288234003, 0.9980164170265072299, 0.9989929497241910594, 0.9999694824218750000 ),
 .UNSPECIFIED. ) ;
#6527 = AXIS2_PLACEMENT_3D ( 'NONE', #16903, #6823, #8423 ) ;
#6528 = ADVANCED_FACE ( 'NONE', ( #8234 ), #6521, .T. ) ;
#6529 = CARTESIAN_POINT ( 'NONE',  ( 2.114046819835705637, 34.88523765466241855, -38.90380387758577996 ) ) ;
#6530 = DIRECTION ( 'NONE',  ( -6.505213034913038160E-19, -3.903127820947822896E-18, -1.000000000000000000 ) ) ;
#6531 = CARTESIAN_POINT ( 'NONE',  ( -18.94034750358418862, 13.51583961449410154, -57.85890765540866454 ) ) ;
#6532 = AXIS2_PLACEMENT_3D ( 'NONE', #8600, #12, #1507 ) ;
#6533 = LINE ( 'NONE', #22349, #15173 ) ;
#6534 = LINE ( 'NONE', #13160, #5927 ) ;
#6535 = ORIENTED_EDGE ( 'NONE', *, *, #8991, .F. ) ;
#6536 = CARTESIAN_POINT ( 'NONE',  ( -31.09841355225989545, 5.093313992686310243, -2.999999999999971578 ) ) ;
#6537 = DIRECTION ( 'NONE',  ( -0.000000000000000000, 1.000000000000000000, -0.000000000000000000 ) ) ;
#6538 = CARTESIAN_POINT ( 'NONE',  ( 35.00000000000000000, -5.000000000000000000, 4.258610482196280173E-15 ) ) ;
#6539 = DIRECTION ( 'NONE',  ( 0.000000000000000000, 0.000000000000000000, 1.000000000000000000 ) ) ;
#6540 = ORIENTED_EDGE ( 'NONE', *, *, #10743, .F. ) ;
#6541 = VECTOR ( 'NONE', #7566, 1000.000000000000000 ) ;
#6542 = FACE_OUTER_BOUND ( 'NONE', #21338, .T. ) ;
#6543 = CARTESIAN_POINT ( 'NONE',  ( 24.10117729468400682, -26.10603996529641080, 3.000000000000047518 ) ) ;
#6544 = AXIS2_PLACEMENT_3D ( 'NONE', #944, #16868, #8159 ) ;
#6545 = DIRECTION ( 'NONE',  ( 6.505213034913038160E-19, 3.903127820947822896E-18, 1.000000000000000000 ) ) ;
#6546 = AXIS2_PLACEMENT_3D ( 'NONE', #12072, #6803, #10330 ) ;
#6547 = ORIENTED_EDGE ( 'NONE', *, *, #22476, .T. ) ;
#6548 = ORIENTED_EDGE ( 'NONE', *, *, #14606, .F. ) ;
#6549 = ADVANCED_FACE ( 'NONE', ( #3079 ), #4582, .T. ) ;
#6550 = VERTEX_POINT ( 'NONE', #20602 ) ;
#6551 = FACE_OUTER_BOUND ( 'NONE', #8338, .T. ) ;
#6552 = CARTESIAN_POINT ( 'NONE',  ( 2.775557561562891351E-14, -2.775557561562891351E-14, 2.999999999999999112 ) ) ;
#6553 = DIRECTION ( 'NONE',  ( 0.000000000000000000, -1.000000000000000000, 0.000000000000000000 ) ) ;
#6554 = ADVANCED_FACE ( 'NONE', ( #18551 ), #18668, .T. ) ;
#6555 = FACE_OUTER_BOUND ( 'NONE', #18849, .T. ) ;
#6556 = CIRCLE ( 'NONE', #8018, 31.50000000000000711 ) ;
#6557 = LINE ( 'NONE', #18811, #13454 ) ;
#6558 = ORIENTED_EDGE ( 'NONE', *, *, #2249, .T. ) ;
#6559 = LINE ( 'NONE', #15464, #5806 ) ;
#6561 = AXIS2_PLACEMENT_3D ( 'NONE', #11707, #14899, #1166 ) ;
#6560 = CARTESIAN_POINT ( 'NONE',  ( 6.696867368503558448E-15, 0.000000000000000000, 48.73397172404481381 ) ) ;
#6562 = EDGE_LOOP ( 'NONE', ( #1993, #18778, #11951, #852, #15513, #17316 ) ) ;
#6563 = DIRECTION ( 'NONE',  ( -1.000000000000000000, -1.208970125616060717E-17, 0.000000000000000000 ) ) ;
#6564 = DIRECTION ( 'NONE',  ( -0.000000000000000000, 1.000000000000000000, -0.000000000000000000 ) ) ;
#6565 = CARTESIAN_POINT ( 'NONE',  ( 90.00000000000000000, 26.00000000000000355, -2.099999999999991651 ) ) ;
#6566 = CARTESIAN_POINT ( 'NONE',  ( 9.226606573888423313, 39.40757736536860278, 54.37932754215746911 ) ) ;
#6567 = ORIENTED_EDGE ( 'NONE', *, *, #10840, .F. ) ;
#6568 = CARTESIAN_POINT ( 'NONE',  ( 34.99999999999980815, 39.97500000000000142, 54.99999999999922551 ) ) ;
#6569 = ADVANCED_FACE ( 'NONE', ( #17161 ), #9726, .F. ) ;
#6570 = VERTEX_POINT ( 'NONE', #9944 ) ;
#6571 = DIRECTION ( 'NONE',  ( -0.000000000000000000, -1.000000000000000000, -0.000000000000000000 ) ) ;
#6572 = CARTESIAN_POINT ( 'NONE',  ( -15.67632863000013188, 36.06985656533339579, 56.80410608597896527 ) ) ;
#6573 = VERTEX_POINT ( 'NONE', #16937 ) ;
#6574 = LINE ( 'NONE', #8399, #14884 ) ;
#6575 = CARTESIAN_POINT ( 'NONE',  ( 6.123233995736766282E-16, -45.00000000000000000, -5.000000000000000000 ) ) ;
#6576 = DIRECTION ( 'NONE',  ( -0.000000000000000000, -1.000000000000000000, -0.000000000000000000 ) ) ;
#6577 = CARTESIAN_POINT ( 'NONE',  ( 17.83526554138365583, 10.93913794110402726, -60.06225905488081906 ) ) ;
#6578 = AXIS2_PLACEMENT_3D ( 'NONE', #3622, #1996, #12629 ) ;
#6579 = VERTEX_POINT ( 'NONE', #16716 ) ;
#6580 = ORIENTED_EDGE ( 'NONE', *, *, #1642, .F. ) ;
#6581 = ORIENTED_EDGE ( 'NONE', *, *, #22627, .F. ) ;
#6582 = DIRECTION ( 'NONE',  ( -0.000000000000000000, -1.000000000000000000, -0.000000000000000000 ) ) ;
#6583 = ORIENTED_EDGE ( 'NONE', *, *, #14854, .T. ) ;
#6584 = PLANE ( 'NONE',  #7414 ) ;
#6585 = LINE ( 'NONE', #20115, #10717 ) ;
#6586 = DIRECTION ( 'NONE',  ( -0.000000000000000000, 1.000000000000000000, -0.000000000000000000 ) ) ;
#6587 = VERTEX_POINT ( 'NONE', #14975 ) ;
#6588 = CYLINDRICAL_SURFACE ( 'NONE', #20073, 3.000000000000000888 ) ;
#6589 = CARTESIAN_POINT ( 'NONE',  ( 2.900269772745152519, 15.21450027326556764, 6.519988159905375724 ) ) ;
#6590 = VERTEX_POINT ( 'NONE', #20848 ) ;
#6591 = CARTESIAN_POINT ( 'NONE',  ( -3.000000000000000000, 16.00000000000000000, 6.485281374238567764 ) ) ;
#6592 = ORIENTED_EDGE ( 'NONE', *, *, #6645, .F. ) ;
#6593 = DIRECTION ( 'NONE',  ( 6.505213034913038160E-19, 3.903127820947822896E-18, 1.000000000000000000 ) ) ;
#6594 = LINE ( 'NONE', #11970, #12368 ) ;
#6595 = LINE ( 'NONE', #4876, #4243 ) ;
#6596 = CARTESIAN_POINT ( 'NONE',  ( -15.27654436812520977, 32.91718622474422773, -59.27094897435731014 ) ) ;
#6597 = EDGE_CURVE ( 'NONE', #4837, #21104, #12122, .T. ) ;
#6598 = DIRECTION ( 'NONE',  ( -0.000000000000000000, -1.000000000000000000, 0.000000000000000000 ) ) ;
#6599 = ORIENTED_EDGE ( 'NONE', *, *, #8202, .T. ) ;
#6600 = ADVANCED_FACE ( 'NONE', ( #22690 ), #11122, .T. ) ;
#6601 = ORIENTED_EDGE ( 'NONE', *, *, #8021, .T. ) ;
#6602 = VERTEX_POINT ( 'NONE', #19352 ) ;
#6603 = EDGE_LOOP ( 'NONE', ( #12285, #12509, #20371 ) ) ;
#6604 = CARTESIAN_POINT ( 'NONE',  ( -22.04638094649398639, 24.21359277922483244, 58.58544938243663580 ) ) ;
#6605 = CYLINDRICAL_SURFACE ( 'NONE', #9622, 19.11328065563151668 ) ;
#6606 = DIRECTION ( 'NONE',  ( 0.000000000000000000, 0.000000000000000000, 1.000000000000000000 ) ) ;
#6607 = CARTESIAN_POINT ( 'NONE',  ( -11.70544581405715512, 40.00000000000000000, 54.22116824785030076 ) ) ;
#6608 = AXIS2_PLACEMENT_3D ( 'NONE', #18848, #20121, #14510 ) ;
#6609 = CARTESIAN_POINT ( 'NONE',  ( 35.00000000000000000, 10.00000000000000000, 41.00000000000002132 ) ) ;
#6610 = EDGE_LOOP ( 'NONE', ( #19157, #21925 ) ) ;
#6611 = CARTESIAN_POINT ( 'NONE',  ( 28.52469787935786982, 7.000000000000000000, -4.095854054471906203 ) ) ;
#6612 = CARTESIAN_POINT ( 'NONE',  ( -8.604786193496984481, 40.00000000000001421, -53.19510613257067178 ) ) ;
#6613 = DIRECTION ( 'NONE',  ( 1.000000000000000000, -1.296372316667914327E-16, 0.000000000000000000 ) ) ;
#6614 = CARTESIAN_POINT ( 'NONE',  ( 34.99999999999980815, 26.00000000000000355, 52.89999999999922409 ) ) ;
#6615 = ORIENTED_EDGE ( 'NONE', *, *, #18744, .T. ) ;
#6616 = CARTESIAN_POINT ( 'NONE',  ( 3.469446951953614189E-15, 38.23275711891355400, 0.000000000000000000 ) ) ;
#6617 = EDGE_CURVE ( 'NONE', #5122, #16507, #2353, .T. ) ;
#6618 = ORIENTED_EDGE ( 'NONE', *, *, #3412, .T. ) ;
#6619 = LINE ( 'NONE', #12332, #14910 ) ;
#6620 = DIRECTION ( 'NONE',  ( 6.505213034913038160E-19, 3.903127820947822896E-18, 1.000000000000000000 ) ) ;
#6621 = DIRECTION ( 'NONE',  ( 0.000000000000000000, 0.000000000000000000, -1.000000000000000000 ) ) ;
#6622 = DIRECTION ( 'NONE',  ( 0.000000000000000000, 1.000000000000000000, 0.000000000000000000 ) ) ;
#6623 = AXIS2_PLACEMENT_3D ( 'NONE', #1657, #18963, #7031 ) ;
#6624 = ORIENTED_EDGE ( 'NONE', *, *, #20999, .F. ) ;
#6625 = ADVANCED_FACE ( 'NONE', ( #2032 ), #1244, .T. ) ;
#6626 = CONICAL_SURFACE ( 'NONE', #1867, 58.99999999999701572, 0.7853981633974447263 ) ;
#6627 = ORIENTED_EDGE ( 'NONE', *, *, #6887, .F. ) ;
#6628 = DIRECTION ( 'NONE',  ( -6.505213034913038160E-19, -3.903127820947822896E-18, -1.000000000000000000 ) ) ;
#6629 = CARTESIAN_POINT ( 'NONE',  ( 35.00000000000058265, 40.00000000000000711, -57.52500000000076597 ) ) ;
#6630 = ORIENTED_EDGE ( 'NONE', *, *, #14554, .F. ) ;
#6631 = DIRECTION ( 'NONE',  ( 1.000000000000000000, 0.000000000000000000, 0.000000000000000000 ) ) ;
#6632 = AXIS2_PLACEMENT_3D ( 'NONE', #13129, #20142, #4446 ) ;
#6633 = EDGE_CURVE ( 'NONE', #15147, #11978, #18072, .T. ) ;
#6634 =( BOUNDED_SURFACE ( )  B_SPLINE_SURFACE ( 3, 2, ( 
 ( #21132, #5434, #7265 ),
 ( #12411, #19422, #10674 ),
 ( #17680, #613, #19980 ),
 ( #19867, #4402, #12623 ),
 ( #490, #4065, #9440 ),
 ( #16075, #21468, #383 ),
 ( #19644, #7600, #11376 ),
 ( #14342, #7377, #7826 ) ),
 .UNSPECIFIED., .F., .F., .F. ) 
 B_SPLINE_SURFACE_WITH_KNOTS ( ( 4, 2, 2, 4 ),
 ( 3, 3 ),
 ( 0.000000000000000000, 0.005619572794280895157, 0.008429359191421343170, 0.01123914558856179031 ),
 ( 0.000000000000000000, 1.000000000000000000 ),
 .UNSPECIFIED. ) 
 GEOMETRIC_REPRESENTATION_ITEM ( )  RATIONAL_B_SPLINE_SURFACE ( (
 ( 1.000000000000000000, 0.7200096751079887447, 1.000000000000000000),
 ( 1.000000000000000000, 0.7496815117894589653, 1.000000000000000000),
 ( 1.000000000000000000, 0.7737746244353003178, 1.000000000000000000),
 ( 1.000000000000000000, 0.8024243379858346792, 1.000000000000000000),
 ( 1.000000000000000000, 0.8107154503869030693, 1.000000000000000000),
 ( 1.000000000000000000, 0.8248921579236677681, 1.000000000000000000),
 ( 1.000000000000000000, 0.8307774003432533139, 1.000000000000000000),
 ( 1.000000000000000000, 0.8354972176269003237, 1.000000000000000000) ) ) 
 REPRESENTATION_ITEM ( '' )  SURFACE ( )  );
#6635 = CARTESIAN_POINT ( 'NONE',  ( 23.49999999999998579, 19.99999999999999645, -105.0010000000000048 ) ) ;
#6636 = LINE ( 'NONE', #8695, #3970 ) ;
#6637 = CARTESIAN_POINT ( 'NONE',  ( -19.59396665412805305, 15.89499847339672556, -60.52448832957815483 ) ) ;
#6638 = DIRECTION ( 'NONE',  ( 1.049727191138618326E-16, -0.5150380749100547106, 0.8571673007021120005 ) ) ;
#6639 = CARTESIAN_POINT ( 'NONE',  ( -13.23602284716360700, 35.01773851406191085, 58.53880247431295203 ) ) ;
#6640 = ORIENTED_EDGE ( 'NONE', *, *, #10054, .F. ) ;
#6641 = DIRECTION ( 'NONE',  ( -0.000000000000000000, -1.000000000000000000, -0.000000000000000000 ) ) ;
#6642 = FILL_AREA_STYLE_COLOUR ( '', #20632 ) ;
#6643 = CARTESIAN_POINT ( 'NONE',  ( -2.783226368218592341E-14, 0.000000000000000000, 47.49736834814792985 ) ) ;
#6644 = EDGE_CURVE ( 'NONE', #4950, #20362, #3761, .T. ) ;
#6645 = EDGE_CURVE ( 'NONE', #21941, #21842, #14040, .T. ) ;
#6646 = DIRECTION ( 'NONE',  ( -0.000000000000000000, 1.000000000000000000, -0.000000000000000000 ) ) ;
#6647 = ORIENTED_EDGE ( 'NONE', *, *, #14045, .F. ) ;
#6648 = DIRECTION ( 'NONE',  ( 0.000000000000000000, 1.000000000000000000, 0.000000000000000000 ) ) ;
#6649 = DIRECTION ( 'NONE',  ( -0.000000000000000000, -1.000000000000000000, -0.000000000000000000 ) ) ;
#6650 = CARTESIAN_POINT ( 'NONE',  ( -32.40961249803547872, 2.422192751863922133, 2.999999999999999112 ) ) ;
#6651 = VECTOR ( 'NONE', #5875, 1000.000000000000000 ) ;
#6652 = EDGE_CURVE ( 'NONE', #22056, #6570, #10279, .T. ) ;
#6653 = ORIENTED_EDGE ( 'NONE', *, *, #19285, .F. ) ;
#6654 = EDGE_CURVE ( 'NONE', #19154, #8041, #20276, .T. ) ;
#6655 = ORIENTED_EDGE ( 'NONE', *, *, #18444, .T. ) ;
#6656 = DIRECTION ( 'NONE',  ( -1.000000000000000000, 1.567804759296643123E-16, 0.000000000000000000 ) ) ;
#6657 = B_SPLINE_CURVE_WITH_KNOTS ( 'NONE', 1,
 ( #9655, #15131 ),
 .UNSPECIFIED., .F., .F.,
 ( 2, 2 ),
 ( 0.000000000000000000, 1.000000000000000000 ),
 .UNSPECIFIED. ) ;
#6658 = CARTESIAN_POINT ( 'NONE',  ( 2.066061548968385786, -1.174227811083158768, 49.70141618117709470 ) ) ;
#6659 = CARTESIAN_POINT ( 'NONE',  ( -1.387778780781445676E-14, 20.00000000000000000, -101.0000000000000284 ) ) ;
#6660 = CARTESIAN_POINT ( 'NONE',  ( 18.43548664438524298, 12.20444905678965242, 60.22785496272550887 ) ) ;
#6661 = ADVANCED_FACE ( 'NONE', ( #8570 ), #13638, .T. ) ;
#6662 = LINE ( 'NONE', #9974, #13839 ) ;
#6663 = ORIENTED_EDGE ( 'NONE', *, *, #13981, .F. ) ;
#6664 = DIRECTION ( 'NONE',  ( 0.000000000000000000, 0.000000000000000000, -1.000000000000000000 ) ) ;
#6665 = DIRECTION ( 'NONE',  ( -0.000000000000000000, -0.000000000000000000, -1.000000000000000000 ) ) ;
#6666 = ORIENTED_EDGE ( 'NONE', *, *, #11764, .F. ) ;
#6667 = DIRECTION ( 'NONE',  ( -0.000000000000000000, -0.000000000000000000, -1.000000000000000000 ) ) ;
#6668 = DIRECTION ( 'NONE',  ( -6.505213034913038160E-19, -3.903127820947822896E-18, -1.000000000000000000 ) ) ;
#6669 = CIRCLE ( 'NONE', #19478, 31.50000000000000000 ) ;
#6670 = CARTESIAN_POINT ( 'NONE',  ( -34.99999999999999289, -4.999999999999997335, -57.00000000000000711 ) ) ;
#6671 = CARTESIAN_POINT ( 'NONE',  ( -34.99999999999999289, -1.000000000000028644, 59.99999999999698019 ) ) ;
#6672 = ORIENTED_EDGE ( 'NONE', *, *, #22688, .T. ) ;
#6673 = CARTESIAN_POINT ( 'NONE',  ( -9.226606582130424172, 39.40757736410211720, -54.37932754532841528 ) ) ;
#6674 = EDGE_LOOP ( 'NONE', ( #20435, #703, #3739, #12573 ) ) ;
#6675 = CYLINDRICAL_SURFACE ( 'NONE', #20729, 25.00000000000000000 ) ;
#6676 = ADVANCED_FACE ( 'NONE', ( #2610, #9139 ), #421, .F. ) ;
#6677 = CARTESIAN_POINT ( 'NONE',  ( -19.46387463785194072, 8.808008015900622212, 57.95411844647836830 ) ) ;
#6678 = ORIENTED_EDGE ( 'NONE', *, *, #15968, .F. ) ;
#6679 = CARTESIAN_POINT ( 'NONE',  ( 2.602085213965210642E-15, 7.999999999999994671, 0.000000000000000000 ) ) ;
#6680 = LINE ( 'NONE', #10322, #19227 ) ;
#6681 = DIRECTION ( 'NONE',  ( 1.000000000000000000, 0.000000000000000000, 0.000000000000000000 ) ) ;
#6682 = ADVANCED_FACE ( 'NONE', ( #19690 ), #4192, .T. ) ;
#6683 = DIRECTION ( 'NONE',  ( -1.000000000000000000, 0.000000000000000000, 0.000000000000000000 ) ) ;
#6684 = EDGE_CURVE ( 'NONE', #16002, #5224, #16112, .T. ) ;
#6685 = ORIENTED_EDGE ( 'NONE', *, *, #2371, .F. ) ;
#6686 = AXIS2_PLACEMENT_3D ( 'NONE', #21775, #6072, #20059 ) ;
#6687 = VECTOR ( 'NONE', #4307, 1000.000000000000000 ) ;
#6688 = ORIENTED_EDGE ( 'NONE', *, *, #1305, .F. ) ;
#6689 = EDGE_CURVE ( 'NONE', #15831, #575, #14779, .T. ) ;
#6690 = ORIENTED_EDGE ( 'NONE', *, *, #20419, .T. ) ;
#6691 = CIRCLE ( 'NONE', #22075, 2.099999999999990763 ) ;
#6692 = ORIENTED_EDGE ( 'NONE', *, *, #3394, .F. ) ;
#6693 = DIRECTION ( 'NONE',  ( -6.505213034913038160E-19, -3.903127820947822896E-18, -1.000000000000000000 ) ) ;
#6694 = CARTESIAN_POINT ( 'NONE',  ( 22.42346072916785360, 20.15694599340440973, 58.66711769948891231 ) ) ;
#6695 = DIRECTION ( 'NONE',  ( -0.000000000000000000, 1.000000000000000000, -0.000000000000000000 ) ) ;
#6696 = EDGE_LOOP ( 'NONE', ( #143, #22633, #13403, #4222 ) ) ;
#6697 = DIRECTION ( 'NONE',  ( -6.505213034913038160E-19, -3.903127820947822896E-18, -1.000000000000000000 ) ) ;
#6698 = CARTESIAN_POINT ( 'NONE',  ( 2.775557561562891351E-14, -2.775557561562891351E-14, 2.999999999999999112 ) ) ;
#6699 = ORIENTED_EDGE ( 'NONE', *, *, #19535, .F. ) ;
#6700 = EDGE_LOOP ( 'NONE', ( #9292, #1761, #17911, #7155 ) ) ;
#6701 = CARTESIAN_POINT ( 'NONE',  ( -15.02862401740807918, -32.75570538720779012, -6.999999999999950262 ) ) ;
#6702 = DIRECTION ( 'NONE',  ( 0.000000000000000000, 0.000000000000000000, -1.000000000000000000 ) ) ;
#6703 = DIRECTION ( 'NONE',  ( 0.000000000000000000, 1.000000000000000000, 0.000000000000000000 ) ) ;
#6704 = CARTESIAN_POINT ( 'NONE',  ( -1.095796999069928335, 39.99285418986146823, 49.56761373141846860 ) ) ;
#6705 = AXIS2_PLACEMENT_3D ( 'NONE', #16325, #21606, #2352 ) ;
#6706 = FACE_OUTER_BOUND ( 'NONE', #13210, .T. ) ;
#6707 = AXIS2_PLACEMENT_3D ( 'NONE', #3255, #15482, #13975 ) ;
#6708 = EDGE_CURVE ( 'NONE', #121, #3042, #16237, .T. ) ;
#6709 = CARTESIAN_POINT ( 'NONE',  ( -11.37797799463864479, 10.21854205506532942, 44.06891764425671454 ) ) ;
#6710 = ORIENTED_EDGE ( 'NONE', *, *, #19425, .F. ) ;
#6711 = ORIENTED_EDGE ( 'NONE', *, *, #12855, .F. ) ;
#6712 = EDGE_CURVE ( 'NONE', #6550, #13970, #7413, .T. ) ;
#6713 = ORIENTED_EDGE ( 'NONE', *, *, #4056, .T. ) ;
#6714 = ORIENTED_EDGE ( 'NONE', *, *, #8177, .F. ) ;
#6715 = CARTESIAN_POINT ( 'NONE',  ( 26.79308242454897382, 16.56444186175074051, -6.999999999999944045 ) ) ;
#6716 = CARTESIAN_POINT ( 'NONE',  ( -11.85401191286884703, -32.83234229683740324, -2.999999999999971578 ) ) ;
#6717 = CIRCLE ( 'NONE', #9636, 22.00000000000000711 ) ;
#6718 = CONICAL_SURFACE ( 'NONE', #7071, 57.00000000000002132, 0.7853981633974437271 ) ;
#6719 = CARTESIAN_POINT ( 'NONE',  ( -10.72803533575910606, 39.99999999999999289, -53.87712872072328452 ) ) ;
#6720 = DIRECTION ( 'NONE',  ( -0.000000000000000000, -1.000000000000000000, -0.000000000000000000 ) ) ;
#6721 = CARTESIAN_POINT ( 'NONE',  ( 6.718896861934306131, 39.70714866090484918, 53.19564681394206218 ) ) ;
#6722 = CIRCLE ( 'NONE', #5615, 22.00000000000000000 ) ;
#6723 = ADVANCED_FACE ( 'NONE', ( #16573 ), #2154, .T. ) ;
#6724 = VERTEX_POINT ( 'NONE', #14386 ) ;
#6725 = FACE_BOUND ( 'NONE', #8721, .T. ) ;
#6726 = CARTESIAN_POINT ( 'NONE',  ( -8.910373547852051601, 39.99999999999999289, -53.30647736630695732 ) ) ;
#6727 = CARTESIAN_POINT ( 'NONE',  ( -89.99999999999701572, -5.000000000000000000, -3.012171160963566127E-14 ) ) ;
#6728 = CARTESIAN_POINT ( 'NONE',  ( 42.50000000000000711, -12.00000000000000000, -54.00000000000000000 ) ) ;
#6729 =( LENGTH_UNIT ( ) NAMED_UNIT ( * ) SI_UNIT ( .MILLI., .METRE. ) );
#6730 = EDGE_CURVE ( 'NONE', #2407, #9840, #14029, .T. ) ;
#6731 = CIRCLE ( 'NONE', #8956, 22.12933039895921539 ) ;
#6732 = EDGE_LOOP ( 'NONE', ( #13549, #6326, #2123, #1421 ) ) ;
#6733 = DIRECTION ( 'NONE',  ( 0.000000000000000000, 0.000000000000000000, -1.000000000000000000 ) ) ;
#6734 = ORIENTED_EDGE ( 'NONE', *, *, #4883, .F. ) ;
#6735 = AXIS2_PLACEMENT_3D ( 'NONE', #2497, #19568, #3994 ) ;
#6736 = LINE ( 'NONE', #10605, #21398 ) ;
#6737 = CARTESIAN_POINT ( 'NONE',  ( -6.699391982050367567, -4.821764332415702903, -49.69317737456919559 ) ) ;
#6738 = FACE_BOUND ( 'NONE', #437, .T. ) ;
#6739 = AXIS2_PLACEMENT_3D ( 'NONE', #20066, #9523, #4257 ) ;
#6740 = ORIENTED_EDGE ( 'NONE', *, *, #3180, .F. ) ;
#6741 = ORIENTED_EDGE ( 'NONE', *, *, #18691, .F. ) ;
#6742 = CARTESIAN_POINT ( 'NONE',  ( -2.085528189144346900, -1.173081074622058351, 49.71451653583131503 ) ) ;
#6743 = AXIS2_PLACEMENT_3D ( 'NONE', #1641, #10865, #12066 ) ;
#6744 = CARTESIAN_POINT ( 'NONE',  ( 27.64365646977290325, 17.09029715894935819, 2.999999999999995559 ) ) ;
#6745 = VERTEX_POINT ( 'NONE', #21629 ) ;
#6746 = EDGE_CURVE ( 'NONE', #20985, #9978, #6161, .T. ) ;
#6747 = CARTESIAN_POINT ( 'NONE',  ( 14.76055860720887658, 17.30233064284066558, 45.72055682016589628 ) ) ;
#6748 = VECTOR ( 'NONE', #17135, 1000.000000000000000 ) ;
#6749 = PRODUCT_RELATED_PRODUCT_CATEGORY ( 'part', '', ( #2548 ) ) ;
#6750 = CARTESIAN_POINT ( 'NONE',  ( -13.00000000000000178, 20.00000000000000000, -11.32475165290611407 ) ) ;
#6751 = CARTESIAN_POINT ( 'NONE',  ( 42.50000000000000000, 10.00000000000000000, 47.49999999999999289 ) ) ;
#6752 = CARTESIAN_POINT ( 'NONE',  ( -19.87880993181333267, 17.63198765388839462, -60.59324977527813871 ) ) ;
#6753 = CIRCLE ( 'NONE', #16626, 2.499999999999995115 ) ;
#6754 = CARTESIAN_POINT ( 'NONE',  ( -2.081668171172227205E-14, 40.00000000000002132, 48.73397172404484223 ) ) ;
#6755 = ADVANCED_FACE ( 'NONE', ( #5925 ), #13005, .T. ) ;
#6756 = CARTESIAN_POINT ( 'NONE',  ( -15.40035801025640616, 32.79675990107260475, 56.74176776513680664 ) ) ;
#6757 = ORIENTED_EDGE ( 'NONE', *, *, #15461, .F. ) ;
#6758 = CARTESIAN_POINT ( 'NONE',  ( 12.06668108811419238, 28.91809087000032363, 44.43106897542664058 ) ) ;
#6759 = PRESENTATION_STYLE_ASSIGNMENT (( #22463 ) ) ;
#6760 = CARTESIAN_POINT ( 'NONE',  ( -36.06598984771573413, 10.00000000000000000, 48.42385786802029912 ) ) ;
#6761 = DIRECTION ( 'NONE',  ( -0.000000000000000000, 1.000000000000000000, -0.000000000000000000 ) ) ;
#6762 = ORIENTED_EDGE ( 'NONE', *, *, #6366, .T. ) ;
#6763 = DIRECTION ( 'NONE',  ( 0.000000000000000000, 0.000000000000000000, -1.000000000000000000 ) ) ;
#6764 = DIRECTION ( 'NONE',  ( -0.000000000000000000, 1.000000000000000000, -0.000000000000000000 ) ) ;
#6765 = B_SPLINE_CURVE_WITH_KNOTS ( 'NONE', 3,
 ( #16096, #404, #7513, #5796, #21958, #21843 ),
 .UNSPECIFIED., .F., .F.,
 ( 4, 2, 4 ),
 ( 0.000000000000000000, 0.002641318319679887301, 0.005282636639359774601 ),
 .UNSPECIFIED. ) ;
#6766 = AXIS2_PLACEMENT_3D ( 'NONE', #17264, #10495, #13927 ) ;
#6767 = EDGE_CURVE ( 'NONE', #17046, #11670, #19905, .T. ) ;
#6768 = EDGE_LOOP ( 'NONE', ( #12967, #20749, #12741, #13414 ) ) ;
#6769 = PRODUCT_CONTEXT ( 'NONE', #22052, 'mechanical' ) ;
#6770 = EDGE_CURVE ( 'NONE', #6061, #14915, #11309, .T. ) ;
#6771 = EDGE_LOOP ( 'NONE', ( #7631, #2894, #9433, #2605 ) ) ;
#6772 = DIRECTION ( 'NONE',  ( 8.659560562354932858E-17, 0.7071067811865474617, -0.7071067811865474617 ) ) ;
#6773 = CARTESIAN_POINT ( 'NONE',  ( 5.275737522157127195E-15, 12.49999999999999645, 0.000000000000000000 ) ) ;
#6774 = AXIS2_PLACEMENT_3D ( 'NONE', #8362, #3210, #17170 ) ;
#6775 = DIRECTION ( 'NONE',  ( 0.000000000000000000, 0.000000000000000000, 1.000000000000000000 ) ) ;
#6776 = CARTESIAN_POINT ( 'NONE',  ( -34.99999999999999289, 1.000000000000044187, -3.012171160963566127E-14 ) ) ;
#6777 = DIRECTION ( 'NONE',  ( 0.000000000000000000, -1.000000000000000000, 0.000000000000000000 ) ) ;
#6778 = ORIENTED_EDGE ( 'NONE', *, *, #15566, .F. ) ;
#6779 = CARTESIAN_POINT ( 'NONE',  ( -10.70799354677365400, 35.16985127952393242, -1.999999999999977573 ) ) ;
#6780 = CARTESIAN_POINT ( 'NONE',  ( -17.32050807568873196, -25.00000000000000000, 9.999999999999772626 ) ) ;
#6781 = ORIENTED_EDGE ( 'NONE', *, *, #11725, .F. ) ;
#6782 = CARTESIAN_POINT ( 'NONE',  ( -1.387778780781445676E-14, 20.00000000000000000, 98.00000000000000000 ) ) ;
#6783 = AXIS2_PLACEMENT_3D ( 'NONE', #11965, #11847, #3275 ) ;
#6784 = CARTESIAN_POINT ( 'NONE',  ( 3.469446951953614189E-15, 6.776263578034402713E-17, 0.000000000000000000 ) ) ;
#6785 = CARTESIAN_POINT ( 'NONE',  ( -27.84804035626026320, 24.75236754129139882, -6.999999999999964473 ) ) ;
#6786 = DIRECTION ( 'NONE',  ( -0.000000000000000000, 1.000000000000000000, -0.000000000000000000 ) ) ;
#6787 = ORIENTED_EDGE ( 'NONE', *, *, #20750, .T. ) ;
#6788 = LINE ( 'NONE', #20326, #17431 ) ;
#6789 = CARTESIAN_POINT ( 'NONE',  ( 1.045712755958760010, 0.02735658877310587211, -49.70560592369783848 ) ) ;
#6790 = ORIENTED_EDGE ( 'NONE', *, *, #2266, .T. ) ;
#6791 = CARTESIAN_POINT ( 'NONE',  ( -32.09841355225981374, 5.093313992686310243, -7.000000000000006217 ) ) ;
#6792 = CARTESIAN_POINT ( 'NONE',  ( 0.6841746959067585010, 36.75746821813302745, -2.800654218530457484 ) ) ;
#6793 = CARTESIAN_POINT ( 'NONE',  ( 1.010906942018275689, 35.52192638951967041, 3.000000000000061284 ) ) ;
#6794 = AXIS2_PLACEMENT_3D ( 'NONE', #18113, #9299, #20071 ) ;
#6795 = AXIS2_PLACEMENT_3D ( 'NONE', #20466, #13787, #6480 ) ;
#6796 = FACE_OUTER_BOUND ( 'NONE', #8539, .T. ) ;
#6797 = EDGE_CURVE ( 'NONE', #12588, #5844, #19916, .T. ) ;
#6798 = AXIS2_PLACEMENT_3D ( 'NONE', #5885, #16178, #14112 ) ;
#6799 = EDGE_LOOP ( 'NONE', ( #21845, #22689, #12168, #8121 ) ) ;
#6800 = AXIS2_PLACEMENT_3D ( 'NONE', #12776, #5803, #72 ) ;
#6801 = ORIENTED_EDGE ( 'NONE', *, *, #3044, .F. ) ;
#6802 = ORIENTED_EDGE ( 'NONE', *, *, #6240, .F. ) ;
#6804 = EDGE_CURVE ( 'NONE', #1088, #18716, #20283, .T. ) ;
#6803 = DIRECTION ( 'NONE',  ( 0.000000000000000000, -1.000000000000000000, 0.000000000000000000 ) ) ;
#6805 = ADVANCED_FACE ( 'NONE', ( #19799 ), #14725, .T. ) ;
#6806 = EDGE_CURVE ( 'NONE', #21191, #11348, #7845, .T. ) ;
#6807 = ORIENTED_EDGE ( 'NONE', *, *, #11835, .T. ) ;
#6808 = CARTESIAN_POINT ( 'NONE',  ( -13.00000000000011546, 42.51666049839536043, -105.0000000000000142 ) ) ;
#6809 = CARTESIAN_POINT ( 'NONE',  ( 12.23364788621108090, 38.77571842908469080, 55.51446324382119002 ) ) ;
#6810 = CARTESIAN_POINT ( 'NONE',  ( -35.00000000000000000, 40.00000000000000000, 1.387778780781445676E-14 ) ) ;
#6811 = ORIENTED_EDGE ( 'NONE', *, *, #10940, .F. ) ;
#6812 = FACE_OUTER_BOUND ( 'NONE', #12019, .T. ) ;
#6813 = CARTESIAN_POINT ( 'NONE',  ( -5.422702462874739560, 6.007396227957873869, 40.31673423471877271 ) ) ;
#6814 = ORIENTED_EDGE ( 'NONE', *, *, #7644, .F. ) ;
#6815 = AXIS2_PLACEMENT_3D ( 'NONE', #4396, #16528, #5768 ) ;
#6816 = AXIS2_PLACEMENT_3D ( 'NONE', #5436, #19196, #10463 ) ;
#6817 = VECTOR ( 'NONE', #7039, 1000.000000000000000 ) ;
#6818 = CARTESIAN_POINT ( 'NONE',  ( -34.74700806321096280, 12.00937115242622966, -2.800654218530460593 ) ) ;
#6819 = CARTESIAN_POINT ( 'NONE',  ( -3.578893495154609069E-15, -4.765964690024343753, -45.28512947536507482 ) ) ;
#6820 = ORIENTED_EDGE ( 'NONE', *, *, #15769, .T. ) ;
#6821 = CARTESIAN_POINT ( 'NONE',  ( 7.555723902514645651, 38.52224445567463817, -55.93227658743223429 ) ) ;
#6822 = ADVANCED_FACE ( 'NONE', ( #20024 ), #9679, .T. ) ;
#6823 = DIRECTION ( 'NONE',  ( -0.000000000000000000, 1.000000000000000000, -0.000000000000000000 ) ) ;
#6824 = CARTESIAN_POINT ( 'NONE',  ( 2.775557561562891351E-14, 2.775557561562891351E-14, 5.750000000000001776 ) ) ;
#6825 = CARTESIAN_POINT ( 'NONE',  ( 2.220446049250313081E-13, 2.775557561562891351E-14, -2.800654218530485018 ) ) ;
#6826 = CIRCLE ( 'NONE', #2050, 4.000000000000000000 ) ;
#6827 = DIRECTION ( 'NONE',  ( 1.000000000000000000, 0.000000000000000000, 0.000000000000000000 ) ) ;
#6828 = CARTESIAN_POINT ( 'NONE',  ( -1.010906942018023225, -35.52192638951984804, 3.000000000000060840 ) ) ;
#6829 = AXIS2_PLACEMENT_3D ( 'NONE', #15245, #4743, #11711 ) ;
#6830 = AXIS2_PLACEMENT_3D ( 'NONE', #21065, #9144, #543 ) ;
#6831 = AXIS2_PLACEMENT_3D ( 'NONE', #4851, #3248, #11821 ) ;
#6832 = EDGE_LOOP ( 'NONE', ( #18506, #6999, #4153, #3142 ) ) ;
#6833 = CIRCLE ( 'NONE', #1696, 8.999999999999998224 ) ;
#6834 = EDGE_LOOP ( 'NONE', ( #17243, #16439, #10778, #13225 ) ) ;
#6835 = VERTEX_POINT ( 'NONE', #16808 ) ;
#6836 = ORIENTED_EDGE ( 'NONE', *, *, #97, .F. ) ;
#6837 = DIRECTION ( 'NONE',  ( -6.505213034913038160E-19, -3.903127820947822896E-18, -1.000000000000000000 ) ) ;
#6838 = AXIS2_PLACEMENT_3D ( 'NONE', #14614, #5919, #2490 ) ;
#6839 = CARTESIAN_POINT ( 'NONE',  ( -1.387778780781445518E-14, 20.00000000000000355, -102.0000000000000142 ) ) ;
#6840 = LINE ( 'NONE', #10366, #10899 ) ;
#6841 = CARTESIAN_POINT ( 'NONE',  ( 4.435586171696086488, 39.87782507471364823, 51.86130716576708011 ) ) ;
#6842 = ADVANCED_FACE ( 'NONE', ( #995 ), #20139, .T. ) ;
#6843 = EDGE_CURVE ( 'NONE', #12187, #6131, #9701, .T. ) ;
#6844 = ORIENTED_EDGE ( 'NONE', *, *, #1467, .F. ) ;
#6845 = FACE_OUTER_BOUND ( 'NONE', #7681, .T. ) ;
#6846 = CARTESIAN_POINT ( 'NONE',  ( -0.3946983151935553602, 40.00000000000000000, -48.99018270876789671 ) ) ;
#6847 = CARTESIAN_POINT ( 'NONE',  ( -3.469446951953614189E-14, -3.999999999999985345, 48.73397172404114031 ) ) ;
#6848 = FACE_OUTER_BOUND ( 'NONE', #4910, .T. ) ;
#6849 = VECTOR ( 'NONE', #14663, 1000.000000000000000 ) ;
#6850 = DIRECTION ( 'NONE',  ( 6.505213034913038160E-19, 3.903127820947822896E-18, 1.000000000000000000 ) ) ;
#6851 = ORIENTED_EDGE ( 'NONE', *, *, #6852, .F. ) ;
#6852 = EDGE_CURVE ( 'NONE', #18279, #19756, #1213, .T. ) ;
#6853 = CARTESIAN_POINT ( 'NONE',  ( -19.29031483250425438, 25.30268833713983412, 60.44930483060160498 ) ) ;
#6854 = AXIS2_PLACEMENT_3D ( 'NONE', #21348, #382, #263 ) ;
#6855 = ORIENTED_EDGE ( 'NONE', *, *, #12170, .F. ) ;
#6856 = DIRECTION ( 'NONE',  ( 0.000000000000000000, 1.000000000000000000, 0.000000000000000000 ) ) ;
#6857 = CARTESIAN_POINT ( 'NONE',  ( -34.99999999999999289, 0.000000000000000000, -54.99999999999705125 ) ) ;
#6858 = CARTESIAN_POINT ( 'NONE',  ( -35.00000000000000000, 13.99999999999999822, 15.00000000000002132 ) ) ;
#6859 = VERTEX_POINT ( 'NONE', #4556 ) ;
#6860 = B_SPLINE_CURVE_WITH_KNOTS ( 'NONE', 3,
 ( #13515, #18808, #6895, #5067, #10304, #4942 ),
 .UNSPECIFIED., .F., .F.,
 ( 4, 2, 4 ),
 ( 0.000000000000000000, 0.2500000000000000000, 0.5000000000000000000 ),
 .UNSPECIFIED. ) ;
#6861 = VECTOR ( 'NONE', #7425, 1000.000000000000000 ) ;
#6862 = ORIENTED_EDGE ( 'NONE', *, *, #22039, .F. ) ;
#6863 = CARTESIAN_POINT ( 'NONE',  ( 5.079212789377870685, -3.097595057472858127, -50.74825967503618784 ) ) ;
#6864 = CARTESIAN_POINT ( 'NONE',  ( 42.49999999999998579, 10.00000000000000000, -47.49999999999997868 ) ) ;
#6865 = VERTEX_POINT ( 'NONE', #6376 ) ;
#6866 = CIRCLE ( 'NONE', #4325, 25.00000000000000000 ) ;
#6867 = AXIS2_PLACEMENT_3D ( 'NONE', #13399, #22025, #22256 ) ;
#6868 = CARTESIAN_POINT ( 'NONE',  ( 5.011587927596622194, 34.16614174687214955, -40.02147800532275568 ) ) ;
#6869 = CARTESIAN_POINT ( 'NONE',  ( -42.49999999999996447, 7.000000000000000000, -45.00000000000000711 ) ) ;
#6870 = CARTESIAN_POINT ( 'NONE',  ( -19.97049456717394378, 21.17381189076418124, -60.61481192459387302 ) ) ;
#6871 = DIRECTION ( 'NONE',  ( 0.000000000000000000, -0.000000000000000000, -1.000000000000000000 ) ) ;
#6872 = AXIS2_PLACEMENT_3D ( 'NONE', #16525, #7368, #3940 ) ;
#6873 = ORIENTED_EDGE ( 'NONE', *, *, #7442, .F. ) ;
#6874 = PLANE ( 'NONE',  #1724 ) ;
#6875 = AXIS2_PLACEMENT_3D ( 'NONE', #18101, #14308, #2417 ) ;
#6876 = CARTESIAN_POINT ( 'NONE',  ( -90.00000000000000000, 28.00000000000000000, -9.108981535246192915E-16 ) ) ;
#6877 = PLANE ( 'NONE',  #10102 ) ;
#6878 = CARTESIAN_POINT ( 'NONE',  ( 34.99999999999980815, 40.00000000000000000, 54.99999999999922551 ) ) ;
#6879 = VECTOR ( 'NONE', #11313, 1000.000000000000114 ) ;
#6880 = ORIENTED_EDGE ( 'NONE', *, *, #20667, .F. ) ;
#6881 = DIRECTION ( 'NONE',  ( 0.000000000000000000, -1.000000000000000000, 0.000000000000000000 ) ) ;
#6882 = DIRECTION ( 'NONE',  ( -1.000000000000000000, -3.564803380056654458E-15, 0.000000000000000000 ) ) ;
#6883 = EDGE_CURVE ( 'NONE', #8806, #2631, #1451, .T. ) ;
#6884 = AXIS2_PLACEMENT_3D ( 'NONE', #13142, #16246, #5837 ) ;
#6885 = ORIENTED_EDGE ( 'NONE', *, *, #17210, .F. ) ;
#6886 = ADVANCED_FACE ( 'NONE', ( #13228 ), #8437, .F. ) ;
#6887 = EDGE_CURVE ( 'NONE', #18451, #7988, #9925, .T. ) ;
#6888 = CIRCLE ( 'NONE', #9447, 2.500000000000002220 ) ;
#6889 = CIRCLE ( 'NONE', #21894, 49.99999999999998579 ) ;
#6890 = SURFACE_STYLE_USAGE ( .BOTH. , #8584 ) ;
#6891 = APPLICATION_PROTOCOL_DEFINITION ( 'draft international standard', 'automotive_design', 1998, #19716 ) ;
#6892 = CIRCLE ( 'NONE', #18612, 0.9999999999999995559 ) ;
#6893 = EDGE_LOOP ( 'NONE', ( #15167, #8674, #10959, #21929, #10474, #15117 ) ) ;
#6894 = CARTESIAN_POINT ( 'NONE',  ( -31.92986134326215719, 18.22261011550257948, -1.999999999999998224 ) ) ;
#6895 = CARTESIAN_POINT ( 'NONE',  ( -2.670518050928090137, 14.42800760928497539, 8.613211112165400252 ) ) ;
#6896 = DIRECTION ( 'NONE',  ( -1.000000000000000000, 0.000000000000000000, 0.000000000000000000 ) ) ;
#6897 = CARTESIAN_POINT ( 'NONE',  ( -7.505578006075205089, 1.461761173328240515, 55.63523492904089096 ) ) ;
#6898 = CARTESIAN_POINT ( 'NONE',  ( -32.75570538720774749, 15.02862401740778786, 2.999999999999995559 ) ) ;
#6899 = ORIENTED_EDGE ( 'NONE', *, *, #4434, .F. ) ;
#6900 = CARTESIAN_POINT ( 'NONE',  ( 7.463862311151453710, 35.99819890246943999, -2.800654218530457484 ) ) ;
#6901 = CARTESIAN_POINT ( 'NONE',  ( 30.48934413892814987, -16.99647590252656570, -2.999999999999971578 ) ) ;
#6902 = VERTEX_POINT ( 'NONE', #22422 ) ;
#6903 = CARTESIAN_POINT ( 'NONE',  ( -25.00000000000000000, -20.00000000000000000, 6.487780019669002523E-15 ) ) ;
#6904 = CARTESIAN_POINT ( 'NONE',  ( 22.34927643452056145, 22.00360349561973194, -58.65118246389015155 ) ) ;
#6905 = DIRECTION ( 'NONE',  ( -0.000000000000000000, -1.000000000000000000, -0.000000000000000000 ) ) ;
#6906 = CARTESIAN_POINT ( 'NONE',  ( 41.39271818392635538, 10.00000000000000000, 5.943569790512533757 ) ) ;
#6907 = CARTESIAN_POINT ( 'NONE',  ( -4.196817137611960291, 39.89217750879657842, -51.71303688781891594 ) ) ;
#6908 = EDGE_CURVE ( 'NONE', #1434, #19293, #13458, .T. ) ;
#6909 = AXIS2_PLACEMENT_3D ( 'NONE', #12215, #19100, #10485 ) ;
#6910 = EDGE_LOOP ( 'NONE', ( #22686, #3922, #18577, #2205 ) ) ;
#6911 = DIRECTION ( 'NONE',  ( 0.000000000000000000, 0.000000000000000000, 1.000000000000000000 ) ) ;
#6912 = CARTESIAN_POINT ( 'NONE',  ( -12.59807286780803359, 38.55590838447053414, 55.66678043528293784 ) ) ;
#6913 = ORIENTED_EDGE ( 'NONE', *, *, #740, .F. ) ;
#6914 = DIRECTION ( 'NONE',  ( 1.000000000000000000, 0.000000000000000000, 0.000000000000000000 ) ) ;
#6915 = DIRECTION ( 'NONE',  ( 0.000000000000000000, 0.000000000000000000, -1.000000000000000000 ) ) ;
#6916 = DIRECTION ( 'NONE',  ( 8.659560562354932858E-17, 0.7071067811865474617, -0.7071067811865474617 ) ) ;
#6917 = ADVANCED_FACE ( 'NONE', ( #22082 ), #19886, .F. ) ;
#6918 = CIRCLE ( 'NONE', #22664, 19.11328065563151668 ) ;
#6919 = DIRECTION ( 'NONE',  ( 0.000000000000000000, 0.000000000000000000, -1.000000000000000000 ) ) ;
#6920 = ORIENTED_EDGE ( 'NONE', *, *, #13041, .F. ) ;
#6921 = EDGE_CURVE ( 'NONE', #928, #20565, #17300, .T. ) ;
#6922 = EDGE_LOOP ( 'NONE', ( #4076, #10869, #17083, #18422 ) ) ;
#6923 = CONICAL_SURFACE ( 'NONE', #19372, 39.00000000000001421, 0.7853981633974447263 ) ;
#6924 = ORIENTED_EDGE ( 'NONE', *, *, #21793, .T. ) ;
#6925 = ORIENTED_EDGE ( 'NONE', *, *, #22440, .T. ) ;
#6926 = FACE_OUTER_BOUND ( 'NONE', #11165, .T. ) ;
#6927 = CARTESIAN_POINT ( 'NONE',  ( 18.83430946916724835, 32.25183488571027368, 57.78319592314319664 ) ) ;
#6928 = CARTESIAN_POINT ( 'NONE',  ( 8.194251295035146043, 39.99999999999999289, -53.04030059599973157 ) ) ;
#6929 = CARTESIAN_POINT ( 'NONE',  ( 2.321955323317326236, 40.00000000000000711, 50.16149361573952348 ) ) ;
#6930 = ORIENTED_EDGE ( 'NONE', *, *, #182, .F. ) ;
#6931 = CARTESIAN_POINT ( 'NONE',  ( 8.326672684688674053E-14, -28.00000000000013500, 2.999999999999995559 ) ) ;
#6932 = CARTESIAN_POINT ( 'NONE',  ( -1.838758599476153277, 5.110847757086119714, 38.90097524723617539 ) ) ;
#6933 = ORIENTED_EDGE ( 'NONE', *, *, #13188, .F. ) ;
#6934 = CARTESIAN_POINT ( 'NONE',  ( 2.602085213965210642E-15, 0.000000000000000000, 19.00000000000000355 ) ) ;
#6935 = ORIENTED_EDGE ( 'NONE', *, *, #4880, .T. ) ;
#6936 = EDGE_CURVE ( 'NONE', #21565, #6573, #2833, .T. ) ;
#6937 = CARTESIAN_POINT ( 'NONE',  ( 2.605854907981524526, 34.77417319504201032, 39.07589943342649974 ) ) ;
#6938 = ORIENTED_EDGE ( 'NONE', *, *, #8479, .F. ) ;
#6939 = DIRECTION ( 'NONE',  ( 0.000000000000000000, 0.000000000000000000, 1.000000000000000000 ) ) ;
#6940 = CARTESIAN_POINT ( 'NONE',  ( 35.00000000000000000, 2.142135623730931471, 4.258610482196280173E-15 ) ) ;
#6941 = CARTESIAN_POINT ( 'NONE',  ( -2.217097371002125339, 39.97039923937872885, 50.37983947592398692 ) ) ;
#6942 = CIRCLE ( 'NONE', #9503, 2.099999999999997868 ) ;
#6943 = CARTESIAN_POINT ( 'NONE',  ( 13.85640646055130709, 1.500000000000004885, -8.000000000000097700 ) ) ;
#6944 = DIRECTION ( 'NONE',  ( 6.505213034913038160E-19, 3.903127820947822896E-18, 1.000000000000000000 ) ) ;
#6945 = EDGE_CURVE ( 'NONE', #4146, #19820, #8900, .T. ) ;
#6946 = DIRECTION ( 'NONE',  ( -6.505213034913038160E-19, -3.903127820947822896E-18, -1.000000000000000000 ) ) ;
#6947 = ORIENTED_EDGE ( 'NONE', *, *, #7964, .F. ) ;
#6948 = ORIENTED_EDGE ( 'NONE', *, *, #6421, .F. ) ;
#6949 = EDGE_CURVE ( 'NONE', #599, #21858, #12911, .T. ) ;
#6950 = VERTEX_POINT ( 'NONE', #10029 ) ;
#6951 = EDGE_LOOP ( 'NONE', ( #10202, #13480, #22293, #16347, #5814 ) ) ;
#6952 = CARTESIAN_POINT ( 'NONE',  ( -14.30046708970334635, 2.690036953688593524, 56.32185947139072368 ) ) ;
#6953 = CARTESIAN_POINT ( 'NONE',  ( -12.24744603030441148, 40.00000000000000000, 54.43639671998950291 ) ) ;
#6954 = CIRCLE ( 'NONE', #1098, 2.099999999999997868 ) ;
#6955 = EDGE_CURVE ( 'NONE', #12492, #6587, #4669, .T. ) ;
#6956 = CARTESIAN_POINT ( 'NONE',  ( 35.00000000000001421, 5.000000000000000000, 10.00000000000000000 ) ) ;
#6957 = CARTESIAN_POINT ( 'NONE',  ( -14.29266125237886520, 28.07080038625062102, -2.999999999999978240 ) ) ;
#6958 = CARTESIAN_POINT ( 'NONE',  ( 0.1259700001978051875, 39.99990731386942144, 48.83178812613451214 ) ) ;
#6959 = ADVANCED_FACE ( 'NONE', ( #15172 ), #1332, .T. ) ;
#6960 = ORIENTED_EDGE ( 'NONE', *, *, #12490, .F. ) ;
#6961 = CARTESIAN_POINT ( 'NONE',  ( -20.00948735876860596, -24.79619811426206510, 2.999999999999995559 ) ) ;
#6962 = CARTESIAN_POINT ( 'NONE',  ( -9.741231317622572661, 40.00000000000000711, -53.58312282093140055 ) ) ;
#6963 = DIRECTION ( 'NONE',  ( -1.296372316667914327E-16, -1.000000000000000000, 0.000000000000000000 ) ) ;
#6964 = CARTESIAN_POINT ( 'NONE',  ( 11.49398617737438499, 39.99999999999999289, -54.13866599136454028 ) ) ;
#6965 = AXIS2_PLACEMENT_3D ( 'NONE', #15797, #5605, #2061 ) ;
#6966 = ORIENTED_EDGE ( 'NONE', *, *, #2962, .T. ) ;
#6967 = CYLINDRICAL_SURFACE ( 'NONE', #8070, 3.000000000000002665 ) ;
#6968 = DIRECTION ( 'NONE',  ( 0.000000000000000000, 1.000000000000000000, 0.000000000000000000 ) ) ;
#6969 = CIRCLE ( 'NONE', #18674, 34.90673715956759082 ) ;
#6970 = DIRECTION ( 'NONE',  ( 0.000000000000000000, 1.000000000000000000, 0.000000000000000000 ) ) ;
#6971 = CARTESIAN_POINT ( 'NONE',  ( -26.00000000000001421, 19.99999999999982947, 100.0000000000000000 ) ) ;
#6972 = ADVANCED_FACE ( 'NONE', ( #22322 ), #6605, .T. ) ;
#6973 = ORIENTED_EDGE ( 'NONE', *, *, #13379, .T. ) ;
#6974 = ORIENTED_EDGE ( 'NONE', *, *, #12885, .F. ) ;
#6975 = VERTEX_POINT ( 'NONE', #4889 ) ;
#6976 = DIRECTION ( 'NONE',  ( 0.000000000000000000, 0.000000000000000000, -1.000000000000000000 ) ) ;
#6977 = AXIS2_PLACEMENT_3D ( 'NONE', #4166, #14338, #2326 ) ;
#6978 = EDGE_CURVE ( 'NONE', #3604, #21131, #15570, .T. ) ;
#6979 = CARTESIAN_POINT ( 'NONE',  ( 11.70544581405710893, 39.99999999999998579, -54.22116824785025813 ) ) ;
#6980 = ORIENTED_EDGE ( 'NONE', *, *, #10107, .F. ) ;
#6981 = DIRECTION ( 'NONE',  ( 0.000000000000000000, -0.000000000000000000, -1.000000000000000000 ) ) ;
#6982 = CARTESIAN_POINT ( 'NONE',  ( 4.108808078302957689, 34.46226780860838801, -39.55687577697710111 ) ) ;
#6983 = PLANE ( 'NONE',  #11266 ) ;
#6984 = CARTESIAN_POINT ( 'NONE',  ( -19.34774434964848666, 25.08511355156663569, -60.46357625386933421 ) ) ;
#6985 = CARTESIAN_POINT ( 'NONE',  ( 42.50000000000000711, -5.000000000000000000, -49.60000000000000142 ) ) ;
#6986 = ORIENTED_EDGE ( 'NONE', *, *, #9100, .T. ) ;
#6987 = CARTESIAN_POINT ( 'NONE',  ( 21.05198877411809733, -30.13956425491237567, -2.000000000000005329 ) ) ;
#6988 = FACE_BOUND ( 'NONE', #8101, .T. ) ;
#6989 = CARTESIAN_POINT ( 'NONE',  ( 3.608224830031758756E-13, -2.775557561562891351E-14, -4.999999999999997335 ) ) ;
#6990 = DIRECTION ( 'NONE',  ( -0.8391477167891886468, 0.3845457931435830035, 0.3846500258456568289 ) ) ;
#6991 = VERTEX_POINT ( 'NONE', #11865 ) ;
#6992 = CIRCLE ( 'NONE', #1503, 18.42595423422130452 ) ;
#6993 = FACE_BOUND ( 'NONE', #2212, .T. ) ;
#6994 = DIRECTION ( 'NONE',  ( 0.000000000000000000, 0.000000000000000000, 1.000000000000000000 ) ) ;
#6995 = EDGE_CURVE ( 'NONE', #4971, #22365, #10256, .T. ) ;
#6996 = ORIENTED_EDGE ( 'NONE', *, *, #21917, .F. ) ;
#6997 = B_SPLINE_CURVE_WITH_KNOTS ( 'NONE', 3,
 ( #22651, #11632, #17007, #8199, #18972, #13327, #4659, #22308 ),
 .UNSPECIFIED., .F., .F.,
 ( 4, 2, 2, 4 ),
 ( 0.000000000000000000, 0.002219640113528450250, 0.003329460170292675592, 0.004439280227056901368 ),
 .UNSPECIFIED. ) ;
#6998 = EDGE_CURVE ( 'NONE', #9194, #10478, #16399, .T. ) ;
#6999 = ORIENTED_EDGE ( 'NONE', *, *, #5275, .T. ) ;
#7000 = DIRECTION ( 'NONE',  ( 0.000000000000000000, -0.000000000000000000, 1.000000000000000000 ) ) ;
#7001 = CARTESIAN_POINT ( 'NONE',  ( 6.094635461684753786, 0.8905127700669610569, -54.73853566236119406 ) ) ;
#7002 = DIRECTION ( 'NONE',  ( -0.000000000000000000, -1.000000000000000000, -0.000000000000000000 ) ) ;
#7003 = CARTESIAN_POINT ( 'NONE',  ( 0.000000000000000000, 7.000000000000000000, 0.000000000000000000 ) ) ;
#7004 = ORIENTED_EDGE ( 'NONE', *, *, #22176, .F. ) ;
#7005 = DIRECTION ( 'NONE',  ( -6.505213034913038160E-19, -3.903127820947822896E-18, -1.000000000000000000 ) ) ;
#7006 = DIRECTION ( 'NONE',  ( 6.505213034913038160E-19, 3.903127820947822896E-18, 1.000000000000000000 ) ) ;
#7007 = ORIENTED_EDGE ( 'NONE', *, *, #6908, .T. ) ;
#7008 = CARTESIAN_POINT ( 'NONE',  ( 17.32050807568869644, 1.500000000000015099, 10.00000000000013323 ) ) ;
#7009 = CARTESIAN_POINT ( 'NONE',  ( 21.63981290377902411, 13.82170478134235481, -58.49475859713702874 ) ) ;
#7010 = FACE_OUTER_BOUND ( 'NONE', #2434, .T. ) ;
#7011 = CARTESIAN_POINT ( 'NONE',  ( 8.413264644294047301, 39.99999999999999289, 53.12447867214399366 ) ) ;
#7012 = CARTESIAN_POINT ( 'NONE',  ( 13.75658951623322679, 25.99185038947793203, -45.26303799332215760 ) ) ;
#7013 = VERTEX_POINT ( 'NONE', #20820 ) ;
#7014 = CARTESIAN_POINT ( 'NONE',  ( 2.347663744114436568, 31.41239365194195443, 3.000000000000009770 ) ) ;
#7015 = CARTESIAN_POINT ( 'NONE',  ( -16.23964334364515594, 4.495128156857218116, 56.99255277661112018 ) ) ;
#7016 = ORIENTED_EDGE ( 'NONE', *, *, #12763, .F. ) ;
#7017 = EDGE_CURVE ( 'NONE', #9840, #15288, #13617, .T. ) ;
#7018 = DIRECTION ( 'NONE',  ( -0.000000000000000000, 1.000000000000000000, -0.000000000000000000 ) ) ;
#7019 = CARTESIAN_POINT ( 'NONE',  ( 35.00000000000058265, 40.00000000000000711, -57.52500000000076597 ) ) ;
#7020 = VERTEX_POINT ( 'NONE', #12207 ) ;
#7021 = ORIENTED_EDGE ( 'NONE', *, *, #13765, .T. ) ;
#7022 = ORIENTED_EDGE ( 'NONE', *, *, #16055, .F. ) ;
#7023 = ORIENTED_EDGE ( 'NONE', *, *, #9506, .T. ) ;
#7024 = DIRECTION ( 'NONE',  ( -1.000000000000000000, -1.208970125616060101E-17, 6.505213034913038160E-19 ) ) ;
#7025 = FACE_OUTER_BOUND ( 'NONE', #5491, .T. ) ;
#7026 = AXIS2_PLACEMENT_3D ( 'NONE', #5125, #17476, #3173 ) ;
#7027 = CARTESIAN_POINT ( 'NONE',  ( 5.649796600896712206, 40.00000000000000711, -51.93142838570830122 ) ) ;
#7028 = CARTESIAN_POINT ( 'NONE',  ( 9.741231313988977902, 39.99999999999997868, 53.58312281987703329 ) ) ;
#7029 = EDGE_LOOP ( 'NONE', ( #18861, #4817, #10841, #2496 ) ) ;
#7030 = DIRECTION ( 'NONE',  ( 0.000000000000000000, 1.000000000000000000, 0.000000000000000000 ) ) ;
#7031 = DIRECTION ( 'NONE',  ( 1.000000000000000000, 1.208970125616053475E-17, 0.000000000000000000 ) ) ;
#7032 = VERTEX_POINT ( 'NONE', #3402 ) ;
#7033 = CARTESIAN_POINT ( 'NONE',  ( 35.99819890246974552, -7.463862311151231665, 2.800654218530509443 ) ) ;
#7034 = B_SPLINE_CURVE_WITH_KNOTS ( 'NONE', 3,
 ( #17099, #12065, #22623, #5090 ),
 .UNSPECIFIED., .F., .F.,
 ( 4, 4 ),
 ( 9.545285770394248685E-07, 0.001900595205834785563 ),
 .UNSPECIFIED. ) ;
#7035 = ORIENTED_EDGE ( 'NONE', *, *, #1803, .T. ) ;
#7036 = CARTESIAN_POINT ( 'NONE',  ( -1.387778780781445676E-14, 20.00000000000000000, 102.0000000000000142 ) ) ;
#7037 = ORIENTED_EDGE ( 'NONE', *, *, #8536, .F. ) ;
#7038 = DIRECTION ( 'NONE',  ( -6.505213034913038160E-19, -3.903127820947822896E-18, -1.000000000000000000 ) ) ;
#7039 = DIRECTION ( 'NONE',  ( 1.296372316667914327E-16, 1.000000000000000000, -0.000000000000000000 ) ) ;
#7040 = DIRECTION ( 'NONE',  ( 0.000000000000000000, -0.7071067811865500152, -0.7071067811865450192 ) ) ;
#7041 = EDGE_CURVE ( 'NONE', #3928, #1383, #19506, .T. ) ;
#7042 = CARTESIAN_POINT ( 'NONE',  ( 22.42250004520295192, 20.31170080112650922, 58.66691407552199422 ) ) ;
#7043 = FACE_OUTER_BOUND ( 'NONE', #6910, .T. ) ;
#7044 = VECTOR ( 'NONE', #3431, 1000.000000000000000 ) ;
#7045 = CIRCLE ( 'NONE', #13606, 4.999999999999997335 ) ;
#7046 = CYLINDRICAL_SURFACE ( 'NONE', #20278, 2.500000000000002220 ) ;
#7047 = ORIENTED_EDGE ( 'NONE', *, *, #4570, .T. ) ;
#7048 = EDGE_LOOP ( 'NONE', ( #13630, #22569, #12668, #13186 ) ) ;
#7049 = EDGE_CURVE ( 'NONE', #7098, #3030, #15459, .T. ) ;
#7050 = ORIENTED_EDGE ( 'NONE', *, *, #20302, .F. ) ;
#7051 = EDGE_LOOP ( 'NONE', ( #17936, #20219, #21551, #16822 ) ) ;
#7052 = DIRECTION ( 'NONE',  ( 1.000000000000000000, 0.000000000000000000, 0.000000000000000000 ) ) ;
#7053 = CARTESIAN_POINT ( 'NONE',  ( 18.00000000000035882, -2.753796099301802219E-14, -4.999999999999997335 ) ) ;
#7054 = CYLINDRICAL_SURFACE ( 'NONE', #8714, 19.11328065563151668 ) ;
#7055 = CARTESIAN_POINT ( 'NONE',  ( 0.02110524776262648339, 39.99999746527640809, 48.75039555718117157 ) ) ;
#7056 = ADVANCED_FACE ( 'NONE', ( #21040 ), #21149, .F. ) ;
#7057 = ORIENTED_EDGE ( 'NONE', *, *, #2140, .F. ) ;
#7058 = DIRECTION ( 'NONE',  ( -1.000000000000000000, -1.815202222194848078E-15, 0.000000000000000000 ) ) ;
#7059 = CARTESIAN_POINT ( 'NONE',  ( -7.505578006075234399, 1.461761173328249175, -55.63523492904088386 ) ) ;
#7060 = DIRECTION ( 'NONE',  ( -0.000000000000000000, -1.000000000000000000, -0.000000000000000000 ) ) ;
#7061 = DIRECTION ( 'NONE',  ( 0.000000000000000000, 0.000000000000000000, -1.000000000000000000 ) ) ;
#7062 = VECTOR ( 'NONE', #12092, 1000.000000000000000 ) ;
#7063 = CARTESIAN_POINT ( 'NONE',  ( -17.68684951551754381, 29.34943212427064196, 60.02035230153434497 ) ) ;
#7064 = CARTESIAN_POINT ( 'NONE',  ( -7.464643474138812351, 38.57205640809612390, 54.30629673035977589 ) ) ;
#7065 = CARTESIAN_POINT ( 'NONE',  ( 2.220446049250313081E-13, 2.775557561562891351E-14, -2.800654218530485018 ) ) ;
#7066 = FACE_OUTER_BOUND ( 'NONE', #14925, .T. ) ;
#7067 = EDGE_LOOP ( 'NONE', ( #5451, #5634, #17662, #470 ) ) ;
#7068 = CIRCLE ( 'NONE', #12209, 58.99999999999994316 ) ;
#7069 = EDGE_LOOP ( 'NONE', ( #16875, #6615, #11239 ) ) ;
#7070 = EDGE_CURVE ( 'NONE', #7013, #13252, #7100, .T. ) ;
#7071 = AXIS2_PLACEMENT_3D ( 'NONE', #15682, #10182, #11905 ) ;
#7072 = AXIS2_PLACEMENT_3D ( 'NONE', #21001, #8845, #8618 ) ;
#7073 = ORIENTED_EDGE ( 'NONE', *, *, #11296, .T. ) ;
#7074 = CARTESIAN_POINT ( 'NONE',  ( 5.748506628227421089, -0.6819283742231372347, -52.01451867725467793 ) ) ;
#7075 = DIRECTION ( 'NONE',  ( -1.000000000000000000, -1.208970125616057944E-17, 0.000000000000000000 ) ) ;
#7076 = ADVANCED_FACE ( 'NONE', ( #10695 ), #1678, .F. ) ;
#7077 = EDGE_CURVE ( 'NONE', #2772, #9581, #15841, .T. ) ;
#7078 = ADVANCED_FACE ( 'NONE', ( #5455 ), #8533, .T. ) ;
#7079 = FACE_OUTER_BOUND ( 'NONE', #8434, .T. ) ;
#7080 = AXIS2_PLACEMENT_3D ( 'NONE', #13906, #21031, #1893 ) ;
#7081 = CARTESIAN_POINT ( 'NONE',  ( -10.50000000000012079, 42.51666049839536043, -100.0000000000000000 ) ) ;
#7082 = DIRECTION ( 'NONE',  ( 0.000000000000000000, -1.000000000000000000, 0.000000000000000000 ) ) ;
#7083 = CARTESIAN_POINT ( 'NONE',  ( 27.57461708434186320, -4.862148974673824675, 2.999999999999995559 ) ) ;
#7084 = CARTESIAN_POINT ( 'NONE',  ( -15.00000000000001776, 20.77286304060558564, -45.82575694955838941 ) ) ;
#7085 = PRODUCT_DEFINITION_SHAPE ( 'NONE', 'NONE',  #12887 ) ;
#7086 = AXIS2_PLACEMENT_3D ( 'NONE', #3742, #14482, #19664 ) ;
#7087 = ORIENTED_EDGE ( 'NONE', *, *, #18322, .F. ) ;
#7088 = CARTESIAN_POINT ( 'NONE',  ( 42.50000000000000711, -9.600000000000001421, 47.50000000000000711 ) ) ;
#7089 = CARTESIAN_POINT ( 'NONE',  ( 12.50000000000000888, -20.00000000000000000, -35.35533905932738463 ) ) ;
#7090 = EDGE_CURVE ( 'NONE', #1691, #19883, #20599, .T. ) ;
#7091 = CARTESIAN_POINT ( 'NONE',  ( 25.99999999999998579, 19.99999999999999645, -105.0010000000000048 ) ) ;
#7092 = DIRECTION ( 'NONE',  ( -6.505213034913038160E-19, -3.903127820947822896E-18, -1.000000000000000000 ) ) ;
#7093 = CARTESIAN_POINT ( 'NONE',  ( 12.48541242016037955, 11.67824612544544394, -44.64471390988171606 ) ) ;
#7094 = CONICAL_SURFACE ( 'NONE', #4546, 58.99999999999994316, 0.7853981633974725929 ) ;
#7095 = ORIENTED_EDGE ( 'NONE', *, *, #19323, .F. ) ;
#7096 = LINE ( 'NONE', #7204, #17040 ) ;
#7097 = DIRECTION ( 'NONE',  ( 0.4166911066143242914, 0.000000000000000000, 0.9090481404571101320 ) ) ;
#7098 = VERTEX_POINT ( 'NONE', #7162 ) ;
#7099 = VECTOR ( 'NONE', #11187, 1000.000000000000000 ) ;
#7100 = B_SPLINE_CURVE_WITH_KNOTS ( 'NONE', 3,
 ( #6716, #15519, #5342, #12100 ),
 .UNSPECIFIED., .F., .F.,
 ( 4, 4 ),
 ( 0.001893031756884946092, 0.003808480026563296206 ),
 .UNSPECIFIED. ) ;
#7101 = ORIENTED_EDGE ( 'NONE', *, *, #9476, .F. ) ;
#7102 = CYLINDRICAL_SURFACE ( 'NONE', #14930, 2.099999999999990763 ) ;
#7103 = PLANE ( 'NONE',  #9527 ) ;
#7104 = CARTESIAN_POINT ( 'NONE',  ( 35.00000000000000000, -15.00000000000000000, 15.00000000000002132 ) ) ;
#7105 = ORIENTED_EDGE ( 'NONE', *, *, #12780, .F. ) ;
#7106 = DIRECTION ( 'NONE',  ( -6.505213034913038160E-19, -3.903127820947822896E-18, -1.000000000000000000 ) ) ;
#7107 = CARTESIAN_POINT ( 'NONE',  ( -10.72803533576305846, 40.00000000000000711, 53.87712872072454928 ) ) ;
#7108 = ORIENTED_EDGE ( 'NONE', *, *, #16216, .F. ) ;
#7109 = DIRECTION ( 'NONE',  ( -0.000000000000000000, 1.000000000000000000, -0.000000000000000000 ) ) ;
#7110 = EDGE_CURVE ( 'NONE', #8965, #7701, #13999, .T. ) ;
#7111 = CYLINDRICAL_SURFACE ( 'NONE', #2396, 59.99999999999700862 ) ;
#7112 = APPLICATION_CONTEXT ( 'automotive_design' ) ;
#7113 = DIRECTION ( 'NONE',  ( 0.000000000000000000, 0.000000000000000000, -1.000000000000000000 ) ) ;
#7114 = EDGE_CURVE ( 'NONE', #1508, #18491, #11454, .T. ) ;
#7115 = CARTESIAN_POINT ( 'NONE',  ( -7.262748901058905027, 39.65386577537525170, -53.48190595416691195 ) ) ;
#7116 = ORIENTED_EDGE ( 'NONE', *, *, #5467, .T. ) ;
#7117 = CARTESIAN_POINT ( 'NONE',  ( -24.99999999999999645, 20.00000000000000000, 16.50000000000000355 ) ) ;
#7118 = CIRCLE ( 'NONE', #16252, 15.99999999999998579 ) ;
#7119 = CARTESIAN_POINT ( 'NONE',  ( -6.571663263633261032, 39.72078165228079882, -53.11617171249144320 ) ) ;
#7120 = AXIS2_PLACEMENT_3D ( 'NONE', #5839, #11207, #16485 ) ;
#7121 = ORIENTED_EDGE ( 'NONE', *, *, #4648, .F. ) ;
#7122 = EDGE_CURVE ( 'NONE', #20866, #6550, #17699, .T. ) ;
#7123 = CYLINDRICAL_SURFACE ( 'NONE', #18862, 19.11328065563151668 ) ;
#7124 = LINE ( 'NONE', #8402, #13267 ) ;
#7125 = VERTEX_POINT ( 'NONE', #3637 ) ;
#7126 = ORIENTED_EDGE ( 'NONE', *, *, #8412, .F. ) ;
#7127 = B_SPLINE_CURVE_WITH_KNOTS ( 'NONE', 3,
 ( #22515, #6809, #12400, #21012, #15610, #17222, #19410, #17447, #4976, #13653, #6927, #1535, #5102, #5314, #8519, #21121, #19182, #5422, #6694, #20672, #3375, #15494, #20903, #18957, #11957, #8754, #8631, #10335, #15722, #17334, #17563, #13886, #1872, #5204, #37, #12180, #3489, #8854 ),
 .UNSPECIFIED., .F., .F.,
 ( 4, 2, 2, 2, 2, 2, 2, 2, 2, 2, 2, 2, 2, 2, 2, 2, 2, 2, 4 ),
 ( 0.002265996298495700969, 0.003649092030476653800, 0.005032187762457607065, 0.007798379226419504054, 0.01056457069038139671, 0.01333076215434328936, 0.01609695361830517160, 0.01886314508226705558, 0.02439552801019081313, 0.02577862374217175512, 0.02716171947415269017, 0.02992791093811458455, 0.03131100667009553001, 0.03269410240207647200, 0.03546029386603836292, 0.03822648533000025384, 0.03960958106198120277, 0.04099267679396213782, 0.04652505972188593353 ),
 .UNSPECIFIED. ) ;
#7128 = ORIENTED_EDGE ( 'NONE', *, *, #10883, .T. ) ;
#7129 = EDGE_LOOP ( 'NONE', ( #6640, #791, #6451, #16449 ) ) ;
#7130 = CARTESIAN_POINT ( 'NONE',  ( 35.00000000000000000, -5.000000000000000000, 4.258610482196280173E-15 ) ) ;
#7131 = CIRCLE ( 'NONE', #5684, 57.07106781186551103 ) ;
#7132 = DIRECTION ( 'NONE',  ( 0.000000000000000000, -1.000000000000000000, 0.000000000000000000 ) ) ;
#7133 = EDGE_CURVE ( 'NONE', #6590, #20230, #1901, .T. ) ;
#7134 = DIRECTION ( 'NONE',  ( -0.9659258262890683122, -0.2588190451025209060, 1.182917971378669595E-16 ) ) ;
#7135 = CARTESIAN_POINT ( 'NONE',  ( 4.769735225253079136, 40.00000000000001421, 51.49386052712647199 ) ) ;
#7136 = ORIENTED_EDGE ( 'NONE', *, *, #22522, .T. ) ;
#7137 = DIRECTION ( 'NONE',  ( 0.000000000000000000, 0.000000000000000000, -1.000000000000000000 ) ) ;
#7138 = CARTESIAN_POINT ( 'NONE',  ( -2.095812652544424282, 5.144891695986068214, 38.95253985045413714 ) ) ;
#7139 = ORIENTED_EDGE ( 'NONE', *, *, #1448, .T. ) ;
#7140 = CYLINDRICAL_SURFACE ( 'NONE', #4054, 10.00000000000000178 ) ;
#7141 = FACE_OUTER_BOUND ( 'NONE', #7840, .T. ) ;
#7142 = DIRECTION ( 'NONE',  ( 0.000000000000000000, -1.000000000000000000, 0.000000000000000000 ) ) ;
#7143 = ORIENTED_EDGE ( 'NONE', *, *, #13244, .F. ) ;
#7144 = CARTESIAN_POINT ( 'NONE',  ( 3.604218085003671579, 34.56937985513295786, 39.39148225573723749 ) ) ;
#7145 = ORIENTED_EDGE ( 'NONE', *, *, #5084, .T. ) ;
#7146 = DIRECTION ( 'NONE',  ( -0.000000000000000000, -1.000000000000000000, -0.000000000000000000 ) ) ;
#7147 = CARTESIAN_POINT ( 'NONE',  ( -4.577489642160328387, 39.86955245794722202, 51.95007345451820413 ) ) ;
#7148 = AXIS2_PLACEMENT_3D ( 'NONE', #8697, #15553, #10732 ) ;
#7149 = CARTESIAN_POINT ( 'NONE',  ( 18.05287651232773527, 33.35671069585768578, 57.55759232970982708 ) ) ;
#7150 = FACE_OUTER_BOUND ( 'NONE', #18446, .T. ) ;
#7151 = CIRCLE ( 'NONE', #3877, 17.00000000000000000 ) ;
#7152 = CARTESIAN_POINT ( 'NONE',  ( -1.387778780781445518E-14, 20.00000000000000355, -100.0000000000000000 ) ) ;
#7154 = ORIENTED_EDGE ( 'NONE', *, *, #11663, .F. ) ;
#7153 = ADVANCED_FACE ( 'NONE', ( #166 ), #12425, .T. ) ;
#7155 = ORIENTED_EDGE ( 'NONE', *, *, #5949, .T. ) ;
#7156 = EDGE_LOOP ( 'NONE', ( #1457, #12012 ) ) ;
#7157 = AXIS2_PLACEMENT_3D ( 'NONE', #5305, #7018, #12278 ) ;
#7158 = VECTOR ( 'NONE', #12878, 1000.000000000000000 ) ;
#7159 = ORIENTED_EDGE ( 'NONE', *, *, #5380, .T. ) ;
#7160 = CARTESIAN_POINT ( 'NONE',  ( -13.52717286024091869, 5.231573370294034575, 56.05142967219525474 ) ) ;
#7161 = ADVANCED_FACE ( 'NONE', ( #10817 ), #18276, .T. ) ;
#7162 = CARTESIAN_POINT ( 'NONE',  ( 35.00000000000001421, 1.000000000000044187, -10.00000000000000000 ) ) ;
#7163 = CIRCLE ( 'NONE', #21424, 19.11328065563151668 ) ;
#7164 = ADVANCED_BREP_SHAPE_REPRESENTATION ( '', ( #10851, #18273 ), #20471 ) ;
#7165 = DIRECTION ( 'NONE',  ( -1.000000000000000000, -1.208970125616081209E-17, 0.000000000000000000 ) ) ;
#7166 = CARTESIAN_POINT ( 'NONE',  ( 0.06748077356975319685, 39.99997318472687624, 48.78643326364329624 ) ) ;
#7167 = AXIS2_PLACEMENT_3D ( 'NONE', #16932, #10045, #20494 ) ;
#7168 = ORIENTED_EDGE ( 'NONE', *, *, #11911, .T. ) ;
#7169 = CARTESIAN_POINT ( 'NONE',  ( 33.52953626616048410, 9.708269511265299911, 2.999999999999995559 ) ) ;
#7170 = FACE_OUTER_BOUND ( 'NONE', #7619, .T. ) ;
#7171 = CARTESIAN_POINT ( 'NONE',  ( -12.99999999999980282, -2.516660498395516310, -100.0000000000000000 ) ) ;
#7172 = CARTESIAN_POINT ( 'NONE',  ( -34.99999999999999289, 0.000000000000000000, -3.012171160963566127E-14 ) ) ;
#7173 = CYLINDRICAL_SURFACE ( 'NONE', #20825, 2.500000000000002220 ) ;
#7174 = EDGE_CURVE ( 'NONE', #1538, #10179, #17526, .T. ) ;
#7175 = CARTESIAN_POINT ( 'NONE',  ( -14.64427171882024581, 33.62973864230776400, 59.05294378005811495 ) ) ;
#7176 = AXIS2_PLACEMENT_3D ( 'NONE', #11793, #8145, #14999 ) ;
#7177 = TOROIDAL_SURFACE ( 'NONE', #19997, 34.90673715956759082, 8.750000000000000000 ) ;
#7178 = CIRCLE ( 'NONE', #13014, 34.90673715956759082 ) ;
#7179 = VECTOR ( 'NONE', #6117, 1000.000000000000000 ) ;
#7180 = CARTESIAN_POINT ( 'NONE',  ( -35.00000000000000000, 40.00000000000000000, 1.387778780781445676E-14 ) ) ;
#7181 = DIRECTION ( 'NONE',  ( 0.000000000000000000, 0.000000000000000000, -1.000000000000000000 ) ) ;
#7182 = DIRECTION ( 'NONE',  ( 1.000000000000000000, 0.000000000000000000, 0.000000000000000000 ) ) ;
#7183 = ADVANCED_FACE ( 'NONE', ( #16092 ), #7285, .F. ) ;
#7184 = EDGE_LOOP ( 'NONE', ( #3706, #17509 ) ) ;
#7185 = CIRCLE ( 'NONE', #981, 18.00000000000000000 ) ;
#7186 = ORIENTED_EDGE ( 'NONE', *, *, #21711, .T. ) ;
#7187 = ORIENTED_EDGE ( 'NONE', *, *, #14848, .F. ) ;
#7188 = DIRECTION ( 'NONE',  ( 0.000000000000000000, 0.000000000000000000, -1.000000000000000000 ) ) ;
#7189 = CARTESIAN_POINT ( 'NONE',  ( 10.36558328700349563, 39.99999999999998579, -53.76404159467904265 ) ) ;
#7190 = CIRCLE ( 'NONE', #13770, 57.00000000000002132 ) ;
#7191 = DIRECTION ( 'NONE',  ( -1.000000000000000000, 1.070969311094960327E-14, 0.000000000000000000 ) ) ;
#7192 = CARTESIAN_POINT ( 'NONE',  ( -35.00000000000000711, 0.000000000000000000, -38.99999999999997868 ) ) ;
#7193 = CARTESIAN_POINT ( 'NONE',  ( 3.469446951953614189E-15, 38.23275711891355400, 0.000000000000000000 ) ) ;
#7194 = CARTESIAN_POINT ( 'NONE',  ( -15.24242605747142143, 36.49796895611717673, -56.65858500684275612 ) ) ;
#7195 = FACE_BOUND ( 'NONE', #14076, .T. ) ;
#7196 = AXIS2_PLACEMENT_3D ( 'NONE', #2162, #14735, #9595 ) ;
#7197 = ADVANCED_FACE ( 'NONE', ( #9567 ), #11049, .F. ) ;
#7198 = ORIENTED_EDGE ( 'NONE', *, *, #21648, .F. ) ;
#7199 = FACE_OUTER_BOUND ( 'NONE', #1220, .T. ) ;
#7200 = FACE_BOUND ( 'NONE', #17456, .T. ) ;
#7201 = DIRECTION ( 'NONE',  ( -0.000000000000000000, 1.000000000000000000, -0.000000000000000000 ) ) ;
#7202 = DIRECTION ( 'NONE',  ( -1.000000000000000000, 0.000000000000000000, 0.000000000000000000 ) ) ;
#7203 = ORIENTED_EDGE ( 'NONE', *, *, #16597, .T. ) ;
#7204 = CARTESIAN_POINT ( 'NONE',  ( 0.000000000000000000, -45.00000000000000000, 5.000000000000000000 ) ) ;
#7205 = CIRCLE ( 'NONE', #9042, 19.11328065563150957 ) ;
#7206 = CARTESIAN_POINT ( 'NONE',  ( 3.330669073875469621E-13, -1.110223024625156540E-13, -2.999999999999971578 ) ) ;
#7207 = EDGE_CURVE ( 'NONE', #5841, #9227, #16574, .T. ) ;
#7208 = EDGE_CURVE ( 'NONE', #21245, #22593, #18039, .T. ) ;
#7209 = CIRCLE ( 'NONE', #15244, 3.000000000000002665 ) ;
#7210 = EDGE_CURVE ( 'NONE', #12719, #17759, #4521, .T. ) ;
#7211 = ORIENTED_EDGE ( 'NONE', *, *, #13188, .T. ) ;
#7212 = EDGE_CURVE ( 'NONE', #20078, #12474, #19151, .T. ) ;
#7213 = CONTEXT_DEPENDENT_SHAPE_REPRESENTATION ( #3752, #20301 ) ;
#7214 = ORIENTED_EDGE ( 'NONE', *, *, #17385, .T. ) ;
#7215 = CARTESIAN_POINT ( 'NONE',  ( -17.99999999999963762, -2.565454789329504983E-14, -4.999999999999997335 ) ) ;
#7216 = VECTOR ( 'NONE', #7006, 1000.000000000000000 ) ;
#7217 = CARTESIAN_POINT ( 'NONE',  ( -12.82970538955583706, 1.687462484003148688, 55.75926248610267777 ) ) ;
#7218 = DIRECTION ( 'NONE',  ( 0.000000000000000000, 0.000000000000000000, -1.000000000000000000 ) ) ;
#7219 = DIRECTION ( 'NONE',  ( 1.000000000000000000, 0.000000000000000000, 0.000000000000000000 ) ) ;
#7220 = CIRCLE ( 'NONE', #5778, 22.00000000000000711 ) ;
#7221 = EDGE_LOOP ( 'NONE', ( #19712, #6011, #11047, #17637, #6924, #20472, #10492, #150, #13907 ) ) ;
#7222 = CARTESIAN_POINT ( 'NONE',  ( 12.00937115242647835, 34.74700806321096280, 2.800654218530512551 ) ) ;
#7223 = EDGE_CURVE ( 'NONE', #8088, #13043, #22084, .T. ) ;
#7224 = CARTESIAN_POINT ( 'NONE',  ( -8.923978417722670642, 2.083761144194947512, -56.51262908347766256 ) ) ;
#7225 = ORIENTED_EDGE ( 'NONE', *, *, #1138, .T. ) ;
#7226 = CARTESIAN_POINT ( 'NONE',  ( 14.76298474240519987, 28.95348479018566934, -2.999999999999999112 ) ) ;
#7227 = AXIS2_PLACEMENT_3D ( 'NONE', #19570, #3880, #10613 ) ;
#7228 = CARTESIAN_POINT ( 'NONE',  ( 22.27968669415837155, 17.44229586407517374, -58.63614535158252039 ) ) ;
#7229 = CARTESIAN_POINT ( 'NONE',  ( -34.99999999999980815, 26.00000000000000355, 57.09999999999921982 ) ) ;
#7230 = CARTESIAN_POINT ( 'NONE',  ( 28.06260833510335218, -14.30873905802357271, -7.000000000000006217 ) ) ;
#7231 = ADVANCED_FACE ( 'NONE', ( #17820 ), #12987, .F. ) ;
#7232 = VERTEX_POINT ( 'NONE', #401 ) ;
#7233 = DIRECTION ( 'NONE',  ( 0.000000000000000000, 0.7071067811865435759, 0.7071067811865515695 ) ) ;
#7234 = DIRECTION ( 'NONE',  ( -1.000000000000000000, 0.000000000000000000, 0.000000000000000000 ) ) ;
#7235 = CARTESIAN_POINT ( 'NONE',  ( -4.435586534489145194, 39.87782505388838672, -51.86130739366951303 ) ) ;
#7236 = ORIENTED_EDGE ( 'NONE', *, *, #2467, .T. ) ;
#7237 = VECTOR ( 'NONE', #3686, 1000.000000000000000 ) ;
#7238 = DIRECTION ( 'NONE',  ( 6.505213034913038160E-19, 3.903127820947822896E-18, 1.000000000000000000 ) ) ;
#7239 = DIRECTION ( 'NONE',  ( 0.000000000000000000, 0.5150380749100562650, 0.8571673007021111124 ) ) ;
#7240 = EDGE_CURVE ( 'NONE', #8079, #11670, #18044, .T. ) ;
#7241 = CONICAL_SURFACE ( 'NONE', #20056, 7.500000000000000000, 0.7853981633974447263 ) ;
#7242 = VECTOR ( 'NONE', #19889, 1000.000000000000000 ) ;
#7243 = CIRCLE ( 'NONE', #12369, 1.000000000000000888 ) ;
#7245 = EDGE_CURVE ( 'NONE', #9571, #10118, #11089, .T. ) ;
#7244 = ORIENTED_EDGE ( 'NONE', *, *, #12251, .T. ) ;
#7246 = ADVANCED_FACE ( 'NONE', ( #7509 ), #2475, .T. ) ;
#7247 = VERTEX_POINT ( 'NONE', #4308 ) ;
#7248 = ORIENTED_EDGE ( 'NONE', *, *, #13670, .T. ) ;
#7249 = ORIENTED_EDGE ( 'NONE', *, *, #10047, .F. ) ;
#7250 = CARTESIAN_POINT ( 'NONE',  ( 14.99999999999998579, 20.00000000000000355, -101.0000000000000284 ) ) ;
#7251 = CARTESIAN_POINT ( 'NONE',  ( -19.99999999999998934, -4.500000000000007994, 2.449293598294705724E-15 ) ) ;
#7252 = CARTESIAN_POINT ( 'NONE',  ( 7.892682237755481722, 39.99999999999999289, 52.92195234101908596 ) ) ;
#7253 = AXIS2_PLACEMENT_3D ( 'NONE', #7461, #3476, #17894 ) ;
#7254 = EDGE_CURVE ( 'NONE', #21483, #2902, #7068, .T. ) ;
#7255 = ORIENTED_EDGE ( 'NONE', *, *, #213, .T. ) ;
#7256 = LINE ( 'NONE', #18012, #13820 ) ;
#7257 = CARTESIAN_POINT ( 'NONE',  ( 0.000000000000000000, 0.000000000000000000, 9.068199145005368464E-15 ) ) ;
#7258 = ORIENTED_EDGE ( 'NONE', *, *, #10724, .F. ) ;
#7259 = DIRECTION ( 'NONE',  ( 6.505213034913038160E-19, 3.903127820947822896E-18, 1.000000000000000000 ) ) ;
#7260 = CARTESIAN_POINT ( 'NONE',  ( -19.75454541434355349, 30.69619330606319707, -58.03277863335246423 ) ) ;
#7261 = AXIS2_PLACEMENT_3D ( 'NONE', #21689, #10666, #5881 ) ;
#7262 = VECTOR ( 'NONE', #2220, 1000.000000000000000 ) ;
#7263 = FACE_OUTER_BOUND ( 'NONE', #15492, .T. ) ;
#7264 = ORIENTED_EDGE ( 'NONE', *, *, #11758, .T. ) ;
#7265 = CARTESIAN_POINT ( 'NONE',  ( 7.505578006071305985, 1.461761173326673324, 55.63523492903841117 ) ) ;
#7266 = ORIENTED_EDGE ( 'NONE', *, *, #7313, .T. ) ;
#7267 = CARTESIAN_POINT ( 'NONE',  ( 5.551115123125782702E-14, -1.387778780781445676E-13, -5.749999999999949374 ) ) ;
#7268 = CIRCLE ( 'NONE', #11123, 2.499999999999995115 ) ;
#7269 = CARTESIAN_POINT ( 'NONE',  ( -34.99999999999999289, -4.928932188134504955, -57.07106781186550393 ) ) ;
#7270 = AXIS2_PLACEMENT_3D ( 'NONE', #17758, #21312, #8935 ) ;
#7271 = DIRECTION ( 'NONE',  ( 0.000000000000000000, 0.000000000000000000, 1.000000000000000000 ) ) ;
#7272 = DIRECTION ( 'NONE',  ( -1.000000000000000000, 1.084202172485504434E-16, 0.000000000000000000 ) ) ;
#7273 = DIRECTION ( 'NONE',  ( 1.000000000000000000, 0.000000000000000000, 0.000000000000000000 ) ) ;
#7274 = CARTESIAN_POINT ( 'NONE',  ( 18.94034750358030550, 13.51583961449599336, 57.85890765540172964 ) ) ;
#7275 = CARTESIAN_POINT ( 'NONE',  ( -90.00000000000000000, 28.00000000000000000, -9.108981535246192915E-16 ) ) ;
#7276 = CARTESIAN_POINT ( 'NONE',  ( -26.64693883069154623, -24.43377932785630335, -2.933296326616347205 ) ) ;
#7277 = VECTOR ( 'NONE', #8444, 1000.000000000000000 ) ;
#7278 = VECTOR ( 'NONE', #17303, 1000.000000000000000 ) ;
#7280 = ADVANCED_FACE ( 'NONE', ( #3146 ), #3435, .F. ) ;
#7279 = VERTEX_POINT ( 'NONE', #21840 ) ;
#7281 = ORIENTED_EDGE ( 'NONE', *, *, #594, .T. ) ;
#7282 = VERTEX_POINT ( 'NONE', #4647 ) ;
#7283 = ORIENTED_EDGE ( 'NONE', *, *, #18365, .T. ) ;
#7284 = DIRECTION ( 'NONE',  ( 0.000000000000000000, -1.000000000000000000, 0.000000000000000000 ) ) ;
#7285 = PLANE ( 'NONE',  #16206 ) ;
#7286 = LINE ( 'NONE', #7624, #1492 ) ;
#7287 = DIRECTION ( 'NONE',  ( 6.505213034913038160E-19, 3.903127820947822896E-18, 1.000000000000000000 ) ) ;
#7288 = DIRECTION ( 'NONE',  ( 0.000000000000000000, 0.000000000000000000, -1.000000000000000000 ) ) ;
#7289 = CARTESIAN_POINT ( 'NONE',  ( 2.229105169396924158, 39.97007249071501178, 50.38830863143780903 ) ) ;
#7290 = MECHANICAL_DESIGN_GEOMETRIC_PRESENTATION_REPRESENTATION (  '', ( #8749 ), #19010 ) ;
#7291 = VERTEX_POINT ( 'NONE', #2698 ) ;
#7292 = FACE_OUTER_BOUND ( 'NONE', #1036, .T. ) ;
#7293 = DIRECTION ( 'NONE',  ( 6.505213034913038160E-19, 3.903127820947822896E-18, 1.000000000000000000 ) ) ;
#7294 = CIRCLE ( 'NONE', #16059, 19.11328065563151668 ) ;
#7295 = CARTESIAN_POINT ( 'NONE',  ( 36.54278193890323223, 4.025500340002318822, -2.000000000000005329 ) ) ;
#7296 = LINE ( 'NONE', #7402, #8625 ) ;
#7297 = CARTESIAN_POINT ( 'NONE',  ( -35.00000000000058265, 28.00000000000000000, -52.50000000000076739 ) ) ;
#7298 = EDGE_CURVE ( 'NONE', #728, #2190, #14742, .T. ) ;
#7299 = CARTESIAN_POINT ( 'NONE',  ( 2.220446049250313081E-13, 2.775557561562891351E-14, -2.800654218530485018 ) ) ;
#7300 = CARTESIAN_POINT ( 'NONE',  ( 35.00000000000058265, 40.00000000000000711, -55.00000000000076028 ) ) ;
#7301 = EDGE_CURVE ( 'NONE', #6991, #968, #7802, .T. ) ;
#7302 = CARTESIAN_POINT ( 'NONE',  ( -42.50000000000000711, -12.00000000000000000, -49.60000000000000142 ) ) ;
#7303 = CARTESIAN_POINT ( 'NONE',  ( -23.50000000000001066, 19.99999999999982947, -105.0000000000000142 ) ) ;
#7304 = ORIENTED_EDGE ( 'NONE', *, *, #22658, .F. ) ;
#7305 = ORIENTED_EDGE ( 'NONE', *, *, #13581, .F. ) ;
#7306 = CIRCLE ( 'NONE', #6578, 2.499999999999998668 ) ;
#7307 = EDGE_LOOP ( 'NONE', ( #7690, #14541, #3816, #14206 ) ) ;
#7308 = CARTESIAN_POINT ( 'NONE',  ( 8.306841137978913991, 0.005341471489716420606, -53.48947974212517664 ) ) ;
#7309 = CARTESIAN_POINT ( 'NONE',  ( 13.00000000000024336, -2.516660498395250745, -105.0010000000000048 ) ) ;
#7310 = CIRCLE ( 'NONE', #20130, 4.000000000000001776 ) ;
#7311 = CARTESIAN_POINT ( 'NONE',  ( 5.551115123125782702E-14, -1.387778780781445676E-13, -5.749999999999949374 ) ) ;
#7312 = CARTESIAN_POINT ( 'NONE',  ( -15.61498135782978558, 7.478867266539152681, 59.38575377909880615 ) ) ;
#7313 = EDGE_CURVE ( 'NONE', #13542, #19759, #22296, .T. ) ;
#7314 = CARTESIAN_POINT ( 'NONE',  ( -35.00000000000000000, 0.000000000000000000, 41.00000000000002132 ) ) ;
#7315 = DIRECTION ( 'NONE',  ( -6.505213034913038160E-19, -3.903127820947822896E-18, -1.000000000000000000 ) ) ;
#7316 = VECTOR ( 'NONE', #6392, 1000.000000000000000 ) ;
#7317 = VERTEX_POINT ( 'NONE', #4763 ) ;
#7318 = DIRECTION ( 'NONE',  ( -6.505213034913038160E-19, -3.903127820947822896E-18, -1.000000000000000000 ) ) ;
#7319 = DIRECTION ( 'NONE',  ( 0.000000000000000000, 0.000000000000000000, -1.000000000000000000 ) ) ;
#7320 = DIRECTION ( 'NONE',  ( 0.000000000000000000, 0.000000000000000000, 1.000000000000000000 ) ) ;
#7321 = FACE_OUTER_BOUND ( 'NONE', #7732, .T. ) ;
#7322 = DIRECTION ( 'NONE',  ( 0.000000000000000000, 1.000000000000000000, 0.000000000000000000 ) ) ;
#7323 = EDGE_CURVE ( 'NONE', #6360, #3151, #6003, .T. ) ;
#7324 = VERTEX_POINT ( 'NONE', #14931 ) ;
#7325 = DIRECTION ( 'NONE',  ( 0.000000000000000000, 1.000000000000000000, 0.000000000000000000 ) ) ;
#7326 = DIRECTION ( 'NONE',  ( 0.000000000000000000, -1.000000000000000000, 0.000000000000000000 ) ) ;
#7327 = CARTESIAN_POINT ( 'NONE',  ( -4.936596639065260916, -31.11077005834428277, 2.999999999999999112 ) ) ;
#7328 = AXIS2_PLACEMENT_3D ( 'NONE', #20958, #3549, #10967 ) ;
#7329 = ORIENTED_EDGE ( 'NONE', *, *, #4728, .F. ) ;
#7330 = EDGE_CURVE ( 'NONE', #5420, #1314, #20270, .T. ) ;
#7331 = ITEM_DEFINED_TRANSFORMATION ( 'NONE', 'NONE', #20836,  #18273 ) ;
#7332 = EDGE_LOOP ( 'NONE', ( #9773, #8300, #5096, #18585 ) ) ;
#7333 = CARTESIAN_POINT ( 'NONE',  ( -9.103081159019540181, 0.03030367950604016467, 53.87333532811888404 ) ) ;
#7334 = DIRECTION ( 'NONE',  ( -0.000000000000000000, 1.000000000000000000, -0.000000000000000000 ) ) ;
#7335 = ORIENTED_EDGE ( 'NONE', *, *, #20962, .T. ) ;
#7336 = DIRECTION ( 'NONE',  ( 6.505213034913038160E-19, 3.903127820947822896E-18, 1.000000000000000000 ) ) ;
#7337 = CARTESIAN_POINT ( 'NONE',  ( -6.176809040140576634, 39.99999999999999289, 52.17714401493541487 ) ) ;
#7338 = ORIENTED_EDGE ( 'NONE', *, *, #17720, .T. ) ;
#7339 = EDGE_CURVE ( 'NONE', #13337, #21842, #16893, .T. ) ;
#7341 = EDGE_CURVE ( 'NONE', #16319, #17133, #7444, .T. ) ;
#7340 = CARTESIAN_POINT ( 'NONE',  ( -17.00000000000000711, 0.6398376396478597794, 0.000000000000000000 ) ) ;
#7342 = DIRECTION ( 'NONE',  ( 0.000000000000000000, 0.000000000000000000, 1.000000000000000000 ) ) ;
#7343 = AXIS2_PLACEMENT_3D ( 'NONE', #10336, #11958, #15270 ) ;
#7344 = FACE_OUTER_BOUND ( 'NONE', #16998, .T. ) ;
#7345 = ORIENTED_EDGE ( 'NONE', *, *, #5726, .F. ) ;
#7346 = DIRECTION ( 'NONE',  ( 1.208970125616062874E-17, -1.000000000000000000, 3.903127820947822896E-18 ) ) ;
#7347 = CARTESIAN_POINT ( 'NONE',  ( 12.50000000000000888, 20.00000000000000000, -35.35533905932738463 ) ) ;
#7348 = CARTESIAN_POINT ( 'NONE',  ( -0.3971970637539762872, 39.99908966794054521, -49.04071126575507833 ) ) ;
#7349 = ORIENTED_EDGE ( 'NONE', *, *, #11747, .F. ) ;
#7350 = CARTESIAN_POINT ( 'NONE',  ( 19.05255888325788050, 10.99999999999995381, -5.000000000000004441 ) ) ;
#7351 = CARTESIAN_POINT ( 'NONE',  ( -34.99999999999997868, 0.000000000000000000, 52.49999999999698730 ) ) ;
#7352 = EDGE_CURVE ( 'NONE', #10435, #18025, #6585, .T. ) ;
#7353 = DIRECTION ( 'NONE',  ( 0.000000000000000000, -1.000000000000000000, 0.000000000000000000 ) ) ;
#7354 = ADVANCED_FACE ( 'NONE', ( #6351 ), #19297, .T. ) ;
#7355 = VERTEX_POINT ( 'NONE', #10115 ) ;
#7356 = CIRCLE ( 'NONE', #14289, 34.90673715956759082 ) ;
#7357 = ORIENTED_EDGE ( 'NONE', *, *, #11635, .T. ) ;
#7358 = EDGE_CURVE ( 'NONE', #20463, #10413, #19172, .T. ) ;
#7359 = EDGE_LOOP ( 'NONE', ( #992, #22263, #13814, #15320 ) ) ;
#7360 =( LENGTH_UNIT ( ) NAMED_UNIT ( * ) SI_UNIT ( .MILLI., .METRE. ) );
#7361 = ORIENTED_EDGE ( 'NONE', *, *, #13952, .T. ) ;
#7362 = DIRECTION ( 'NONE',  ( -6.505213034913038160E-19, -3.903127820947822896E-18, -1.000000000000000000 ) ) ;
#7363 = DIRECTION ( 'NONE',  ( 0.000000000000000000, 0.000000000000000000, -1.000000000000000000 ) ) ;
#7364 = CARTESIAN_POINT ( 'NONE',  ( -33.99999999999998579, 6.180736333215580025, 0.000000000000000000 ) ) ;
#7365 = CARTESIAN_POINT ( 'NONE',  ( 4.110274011050107923, 40.00000000000001421, 51.15360529889024832 ) ) ;
#7366 = EDGE_LOOP ( 'NONE', ( #1936, #14220, #9943, #22495 ) ) ;
#7367 = CARTESIAN_POINT ( 'NONE',  ( -35.00000000000058265, 28.00000000000000000, -57.10000000000076170 ) ) ;
#7368 = DIRECTION ( 'NONE',  ( 6.505213034913038160E-19, 3.903127820947822896E-18, 1.000000000000000000 ) ) ;
#7369 = ORIENTED_EDGE ( 'NONE', *, *, #18515, .F. ) ;
#7370 = B_SPLINE_CURVE_WITH_KNOTS ( 'NONE', 3,
 ( #9171, #19605, #14546, #7452 ),
 .UNSPECIFIED., .F., .F.,
 ( 4, 4 ),
 ( 0.001893031756885420322, 0.003808480026563612359 ),
 .UNSPECIFIED. ) ;
#7371 = EDGE_CURVE ( 'NONE', #12420, #16162, #861, .T. ) ;
#7372 = DIRECTION ( 'NONE',  ( -1.000000000000000000, 1.084202172485504927E-16, 0.000000000000000000 ) ) ;
#7373 = CARTESIAN_POINT ( 'NONE',  ( -21.99996130922173876, 24.71724789032313296, -58.57718774367117476 ) ) ;
#7374 = VECTOR ( 'NONE', #2261, 1000.000000000000000 ) ;
#7375 = DIRECTION ( 'NONE',  ( 0.000000000000000000, 0.000000000000000000, -1.000000000000000000 ) ) ;
#7376 = VERTEX_POINT ( 'NONE', #10565 ) ;
#7377 = CARTESIAN_POINT ( 'NONE',  ( -0.2893420571180346235, -0.01224453477246113288, 48.63018218499173884 ) ) ;
#7378 = ORIENTED_EDGE ( 'NONE', *, *, #5943, .T. ) ;
#7379 = CARTESIAN_POINT ( 'NONE',  ( 4.278324951947162447, 39.54020021135892193, -53.33400390259981805 ) ) ;
#7380 = DIRECTION ( 'NONE',  ( -1.000000000000000000, 1.301042606982605814E-16, 0.000000000000000000 ) ) ;
#7381 = EDGE_CURVE ( 'NONE', #18864, #19744, #15383, .T. ) ;
#7382 = DIRECTION ( 'NONE',  ( 0.000000000000000000, 0.000000000000000000, 1.000000000000000000 ) ) ;
#7383 = ORIENTED_EDGE ( 'NONE', *, *, #5167, .T. ) ;
#7384 = CARTESIAN_POINT ( 'NONE',  ( 19.87880993181303779, 17.63198765388676392, 60.59324977527815292 ) ) ;
#7385 = EDGE_CURVE ( 'NONE', #13841, #13545, #8411, .T. ) ;
#7386 = DIRECTION ( 'NONE',  ( 0.000000000000000000, 0.000000000000000000, 1.000000000000000000 ) ) ;
#7387 = LINE ( 'NONE', #9214, #2367 ) ;
#7388 = ORIENTED_EDGE ( 'NONE', *, *, #20076, .F. ) ;
#7389 = VERTEX_POINT ( 'NONE', #3266 ) ;
#7390 = ORIENTED_EDGE ( 'NONE', *, *, #4693, .F. ) ;
#7391 = VERTEX_POINT ( 'NONE', #20789 ) ;
#7392 = DIRECTION ( 'NONE',  ( 0.000000000000000000, 0.000000000000000000, -1.000000000000000000 ) ) ;
#7393 = CARTESIAN_POINT ( 'NONE',  ( -10.80340688051430931, 39.17018323810926006, -54.94414022072520964 ) ) ;
#7394 = LINE ( 'NONE', #5672, #11385 ) ;
#7395 = ORIENTED_EDGE ( 'NONE', *, *, #5963, .T. ) ;
#7396 = CARTESIAN_POINT ( 'NONE',  ( -11.15511648635851039, 39.11609166919295433, -55.07420106208766697 ) ) ;
#7397 = B_SPLINE_CURVE_WITH_KNOTS ( 'NONE', 3,
 ( #5215, #6819, #149, #19077 ),
 .UNSPECIFIED., .F., .F.,
 ( 4, 4 ),
 ( 0.004232217698034760993, 0.004798505571456043728 ),
 .UNSPECIFIED. ) ;
#7398 = CARTESIAN_POINT ( 'NONE',  ( -32.35999952201570551, 1.423424233832487618, -2.999999999999971578 ) ) ;
#7399 = EDGE_LOOP ( 'NONE', ( #7667, #5902, #17929, #19657 ) ) ;
#7400 = DIRECTION ( 'NONE',  ( -0.000000000000000000, 1.000000000000000000, -0.000000000000000000 ) ) ;
#7401 = DIRECTION ( 'NONE',  ( -6.505213034913038160E-19, -3.903127820947822896E-18, -1.000000000000000000 ) ) ;
#7402 = CARTESIAN_POINT ( 'NONE',  ( -5.833333333333339255, 40.00000000000000000, -40.61164310337066041 ) ) ;
#7403 = CARTESIAN_POINT ( 'NONE',  ( -20.00000000000001421, 20.00000000000000000, -60.62177826491068799 ) ) ;
#7404 = EDGE_CURVE ( 'NONE', #17217, #1277, #2706, .T. ) ;
#7405 = CYLINDRICAL_SURFACE ( 'NONE', #10592, 16.49999999999998579 ) ;
#7406 = CARTESIAN_POINT ( 'NONE',  ( 27.84804035626065044, -24.75236754129175765, -2.999999999999971578 ) ) ;
#7407 = FACE_BOUND ( 'NONE', #6696, .T. ) ;
#7408 = EDGE_CURVE ( 'NONE', #17743, #12228, #7127, .T. ) ;
#7409 = CARTESIAN_POINT ( 'NONE',  ( 35.00000000000058265, 40.00000000000000711, -52.47500000000076170 ) ) ;
#7410 = ORIENTED_EDGE ( 'NONE', *, *, #18573, .T. ) ;
#7411 = VERTEX_POINT ( 'NONE', #10449 ) ;
#7412 = ORIENTED_EDGE ( 'NONE', *, *, #1069, .T. ) ;
#7413 = LINE ( 'NONE', #3878, #12567 ) ;
#7414 = AXIS2_PLACEMENT_3D ( 'NONE', #1768, #20560, #15609 ) ;
#7415 = CARTESIAN_POINT ( 'NONE',  ( 2.220446049250313081E-13, -2.498001805406602216E-13, -6.859353255829918616 ) ) ;
#7416 = AXIS2_PLACEMENT_3D ( 'NONE', #3730, #12196, #10682 ) ;
#7417 = ADVANCED_FACE ( 'NONE', ( #7025 ), #12293, .F. ) ;
#7418 = DIRECTION ( 'NONE',  ( 6.505213034913038160E-19, 3.903127820947822896E-18, 1.000000000000000000 ) ) ;
#7419 = CARTESIAN_POINT ( 'NONE',  ( -3.656418565264218934, -37.07861450834831629, -2.999999999999957367 ) ) ;
#7420 = CARTESIAN_POINT ( 'NONE',  ( -34.99999999999999289, 5.000000000000000000, -10.00000000000003020 ) ) ;
#7421 = DIRECTION ( 'NONE',  ( 1.000000000000000000, 0.000000000000000000, 0.000000000000000000 ) ) ;
#7422 = CARTESIAN_POINT ( 'NONE',  ( -42.49999999999996447, 7.000000000000000000, -54.00000000000000711 ) ) ;
#7423 = DIRECTION ( 'NONE',  ( -0.000000000000000000, 1.000000000000000000, -0.000000000000000000 ) ) ;
#7424 = ORIENTED_EDGE ( 'NONE', *, *, #15444, .F. ) ;
#7425 = DIRECTION ( 'NONE',  ( 6.505213034913038160E-19, 3.903127820947822896E-18, 1.000000000000000000 ) ) ;
#7426 = DIRECTION ( 'NONE',  ( 1.000000000000000000, 0.000000000000000000, 0.000000000000000000 ) ) ;
#7427 = FACE_OUTER_BOUND ( 'NONE', #13586, .T. ) ;
#7428 = CARTESIAN_POINT ( 'NONE',  ( 27.57461708434208347, -4.862148974673990764, -5.000000000000004441 ) ) ;
#7429 = DIRECTION ( 'NONE',  ( 0.000000000000000000, -0.000000000000000000, -1.000000000000000000 ) ) ;
#7430 = VERTEX_POINT ( 'NONE', #6050 ) ;
#7431 = AXIS2_PLACEMENT_3D ( 'NONE', #16913, #14954, #3055 ) ;
#7432 = DIRECTION ( 'NONE',  ( -0.000000000000000000, -1.000000000000000000, -0.000000000000000000 ) ) ;
#7433 = DIRECTION ( 'NONE',  ( 0.000000000000000000, 1.000000000000000000, 0.000000000000000000 ) ) ;
#7434 = CIRCLE ( 'NONE', #3424, 2.999999999999999112 ) ;
#7435 = CARTESIAN_POINT ( 'NONE',  ( 16.98435752851229452, 5.286895767878529995, -57.23469700293635753 ) ) ;
#7436 = ORIENTED_EDGE ( 'NONE', *, *, #12082, .T. ) ;
#7437 = EDGE_CURVE ( 'NONE', #16688, #12891, #8914, .T. ) ;
#7438 = LINE ( 'NONE', #14413, #8564 ) ;
#7439 = PRODUCT_DEFINITION ( 'UNKNOWN', '', #4003, #19672 ) ;
#7440 = CONICAL_SURFACE ( 'NONE', #20998, 57.00000000000002132, 0.7853981633974437271 ) ;
#7441 = EDGE_LOOP ( 'NONE', ( #8624, #6920, #14098, #850 ) ) ;
#7442 = EDGE_CURVE ( 'NONE', #6097, #6464, #11431, .T. ) ;
#7443 = FACE_OUTER_BOUND ( 'NONE', #7565, .T. ) ;
#7444 = CIRCLE ( 'NONE', #21358, 31.50000000000001421 ) ;
#7445 = CARTESIAN_POINT ( 'NONE',  ( 35.00000000000000000, -9.000000000000001776, 4.258610482196280173E-15 ) ) ;
#7446 = ORIENTED_EDGE ( 'NONE', *, *, #14657, .T. ) ;
#7447 = DIRECTION ( 'NONE',  ( -1.000000000000000000, 0.000000000000000000, 0.000000000000000000 ) ) ;
#7448 = CONICAL_SURFACE ( 'NONE', #22464, 2.099999999999997868, 1.029744258676653867 ) ;
#7449 = CARTESIAN_POINT ( 'NONE',  ( -9.103081159019568602, 0.03030367950605284896, -53.87333532811888404 ) ) ;
#7450 = ORIENTED_EDGE ( 'NONE', *, *, #4016, .T. ) ;
#7451 = CARTESIAN_POINT ( 'NONE',  ( -6.000000000000000888, -40.00000000000000000, -5.999999999999998224 ) ) ;
#7452 = CARTESIAN_POINT ( 'NONE',  ( -29.33526866242094755, 22.15900668633769044, -2.800654218530477912 ) ) ;
#7453 = CIRCLE ( 'NONE', #11113, 22.00000000000000000 ) ;
#7454 = CARTESIAN_POINT ( 'NONE',  ( 14.99999999999998579, 20.00000000000000355, -45.82575694955836809 ) ) ;
#7455 = CARTESIAN_POINT ( 'NONE',  ( 20.36304159388363644, 24.03323817228475434, -6.999999999999992006 ) ) ;
#7456 = ORIENTED_EDGE ( 'NONE', *, *, #5673, .F. ) ;
#7457 = CARTESIAN_POINT ( 'NONE',  ( -35.00000000000000000, -5.000000000000000000, 1.387778780781445676E-14 ) ) ;
#7458 = CARTESIAN_POINT ( 'NONE',  ( 35.00000000000058265, 39.97500000000000142, -55.00000000000076028 ) ) ;
#7459 = CARTESIAN_POINT ( 'NONE',  ( -6.687085228319380015, 39.71011799691164867, -53.17853451012708632 ) ) ;
#7460 = ORIENTED_EDGE ( 'NONE', *, *, #14498, .F. ) ;
#7461 = CARTESIAN_POINT ( 'NONE',  ( 12.31876324338299078, 30.07487443287970663, 3.000000000000023537 ) ) ;
#7462 = CIRCLE ( 'NONE', #2714, 19.11328065563150957 ) ;
#7463 = ADVANCED_FACE ( 'NONE', ( #18538 ), #1947, .T. ) ;
#7464 = DIRECTION ( 'NONE',  ( -6.505213034913038160E-19, -3.903127820947822896E-18, -1.000000000000000000 ) ) ;
#7465 = DIRECTION ( 'NONE',  ( 0.000000000000000000, 0.000000000000000000, -1.000000000000000000 ) ) ;
#7466 = AXIS2_PLACEMENT_3D ( 'NONE', #7533, #7871, #7755 ) ;
#7467 = EDGE_CURVE ( 'NONE', #3688, #18025, #19900, .T. ) ;
#7468 = CIRCLE ( 'NONE', #20287, 8.999999999999998224 ) ;
#7469 = EDGE_LOOP ( 'NONE', ( #9672, #20120, #4372, #849 ) ) ;
#7470 = ORIENTED_EDGE ( 'NONE', *, *, #10938, .T. ) ;
#7471 = ORIENTED_EDGE ( 'NONE', *, *, #13692, .F. ) ;
#7472 =( NAMED_UNIT ( * ) SI_UNIT ( $, .STERADIAN. ) SOLID_ANGLE_UNIT ( ) );
#7473 = ORIENTED_EDGE ( 'NONE', *, *, #1783, .F. ) ;
#7474 = CARTESIAN_POINT ( 'NONE',  ( -35.00000000000000000, 22.00000000000000355, 2.365113165210053967E-14 ) ) ;
#7475 = DIRECTION ( 'NONE',  ( -0.000000000000000000, -1.000000000000000000, -0.000000000000000000 ) ) ;
#7476 = CARTESIAN_POINT ( 'NONE',  ( -28.88846368933341324, -19.59430950039328678, 2.999999999999995559 ) ) ;
#7477 = DIRECTION ( 'NONE',  ( 0.000000000000000000, 0.000000000000000000, -1.000000000000000000 ) ) ;
#7478 = AXIS2_PLACEMENT_3D ( 'NONE', #5598, #6333, #18821 ) ;
#7479 = ORIENTED_EDGE ( 'NONE', *, *, #10376, .F. ) ;
#7480 = CYLINDRICAL_SURFACE ( 'NONE', #8751, 30.00000000000000000 ) ;
#7481 = DIRECTION ( 'NONE',  ( -0.1421319796954317316, 0.000000000000000000, 0.9898477157360406897 ) ) ;
#7482 = VERTEX_POINT ( 'NONE', #4455 ) ;
#7483 = CARTESIAN_POINT ( 'NONE',  ( 1.045507549828128990, 0.02734584580075648946, 49.70576511417586829 ) ) ;
#7484 = FACE_OUTER_BOUND ( 'NONE', #9650, .T. ) ;
#7485 = CARTESIAN_POINT ( 'NONE',  ( -15.00000000000001421, 20.00000000000000000, 60.00200000000000244 ) ) ;
#7486 = VERTEX_POINT ( 'NONE', #18414 ) ;
#7487 = CARTESIAN_POINT ( 'NONE',  ( -1.387778780781445676E-14, 20.00000000000000000, 98.00000000000000000 ) ) ;
#7488 = VERTEX_POINT ( 'NONE', #2734 ) ;
#7489 = CARTESIAN_POINT ( 'NONE',  ( 1.268121568163980362, 39.97056933375353793, -50.22305475356783688 ) ) ;
#7490 = CARTESIAN_POINT ( 'NONE',  ( -12.99999999999999467, 20.00000000000000000, 11.32475165290612296 ) ) ;
#7491 = CARTESIAN_POINT ( 'NONE',  ( -14.30873905802343415, -28.06260833510307151, -6.999999999999950262 ) ) ;
#7492 = CIRCLE ( 'NONE', #12197, 3.999999999999996447 ) ;
#7493 = FACE_OUTER_BOUND ( 'NONE', #20752, .T. ) ;
#7494 = ORIENTED_EDGE ( 'NONE', *, *, #17293, .F. ) ;
#7495 = CARTESIAN_POINT ( 'NONE',  ( 9.038718750511064215, 40.00000000000000000, -53.35171082564918521 ) ) ;
#7496 = ADVANCED_FACE ( 'NONE', ( #4569 ), #17687, .F. ) ;
#7497 = CARTESIAN_POINT ( 'NONE',  ( 22.35494499951315106, 21.77768233190464287, 58.65240855008568843 ) ) ;
#7498 = CARTESIAN_POINT ( 'NONE',  ( 17.38334492574566070, 30.99230043872318419, -3.000000000000006217 ) ) ;
#7499 = CARTESIAN_POINT ( 'NONE',  ( 8.331955809010596070, 38.18181818181818699, -56.36098470834070895 ) ) ;
#7500 = AXIS2_PLACEMENT_3D ( 'NONE', #14523, #21535, #20156 ) ;
#7501 = EDGE_CURVE ( 'NONE', #9389, #249, #15113, .T. ) ;
#7502 = EDGE_CURVE ( 'NONE', #14282, #17751, #16222, .T. ) ;
#7504 = EDGE_CURVE ( 'NONE', #20345, #4779, #6717, .T. ) ;
#7503 = EDGE_LOOP ( 'NONE', ( #7203, #6885, #14103, #4294 ) ) ;
#7505 = VERTEX_POINT ( 'NONE', #14633 ) ;
#7506 = ORIENTED_EDGE ( 'NONE', *, *, #7919, .T. ) ;
#7507 = ORIENTED_EDGE ( 'NONE', *, *, #2239, .T. ) ;
#7508 = CARTESIAN_POINT ( 'NONE',  ( -24.79619811426206510, 21.00948735876881202, -6.999999999999950262 ) ) ;
#7509 = FACE_OUTER_BOUND ( 'NONE', #7584, .T. ) ;
#7510 = DIRECTION ( 'NONE',  ( -0.000000000000000000, 1.000000000000000000, -0.000000000000000000 ) ) ;
#7511 = EDGE_CURVE ( 'NONE', #16627, #10912, #21737, .T. ) ;
#7512 = ORIENTED_EDGE ( 'NONE', *, *, #1138, .F. ) ;
#7513 = CARTESIAN_POINT ( 'NONE',  ( 8.916870955512969488, 2.080241304160146854, 56.50845996868202548 ) ) ;
#7514 = PLANE ( 'NONE',  #5602 ) ;
#7515 = CIRCLE ( 'NONE', #4588, 34.90673715956759082 ) ;
#7516 = VECTOR ( 'NONE', #18330, 1000.000000000000000 ) ;
#7517 = ORIENTED_EDGE ( 'NONE', *, *, #5227, .T. ) ;
#7518 = DIRECTION ( 'NONE',  ( -1.000000000000000000, 1.264902534566437206E-16, 0.000000000000000000 ) ) ;
#7519 = CARTESIAN_POINT ( 'NONE',  ( -35.00000000000058265, 40.00000000000000000, -55.00000000000076028 ) ) ;
#7520 = CARTESIAN_POINT ( 'NONE',  ( -34.74700806321096280, 12.00937115242622966, -2.800654218530460593 ) ) ;
#7521 = CARTESIAN_POINT ( 'NONE',  ( -10.30713387248692037, 2.842164160680663798, -57.27491564205611496 ) ) ;
#7522 = AXIS2_PLACEMENT_3D ( 'NONE', #17310, #3356, #5295 ) ;
#7523 = DIRECTION ( 'NONE',  ( 0.000000000000000000, -1.000000000000000000, 0.000000000000000000 ) ) ;
#7524 = DIRECTION ( 'NONE',  ( 0.000000000000000000, -0.7071067811867928210, -0.7071067811863022134 ) ) ;
#7525 = DIRECTION ( 'NONE',  ( -0.000000000000000000, 1.000000000000000000, -0.000000000000000000 ) ) ;
#7526 = AXIS2_PLACEMENT_3D ( 'NONE', #19057, #14207, #10652 ) ;
#7527 = ORIENTED_EDGE ( 'NONE', *, *, #18287, .T. ) ;
#7528 = ORIENTED_EDGE ( 'NONE', *, *, #12040, .T. ) ;
#7529 = VECTOR ( 'NONE', #5593, 1000.000000000000000 ) ;
#7530 = ADVANCED_FACE ( 'NONE', ( #18165 ), #11164, .T. ) ;
#7531 = VERTEX_POINT ( 'NONE', #12873 ) ;
#7532 = AXIS2_PLACEMENT_3D ( 'NONE', #21987, #14962, #8004 ) ;
#7533 = CARTESIAN_POINT ( 'NONE',  ( -13.85640646055084702, 1.500000000000008216, 7.999999999999705125 ) ) ;
#7534 = EDGE_CURVE ( 'NONE', #15820, #21174, #15484, .T. ) ;
#7535 = CARTESIAN_POINT ( 'NONE',  ( -35.33352588067087652, -7.094908322883425100, -2.999999999999971578 ) ) ;
#7536 = CYLINDRICAL_SURFACE ( 'NONE', #18318, 1.000000000000000888 ) ;
#7537 = EDGE_CURVE ( 'NONE', #18815, #18105, #8193, .T. ) ;
#7538 = DIRECTION ( 'NONE',  ( -1.000000000000000000, 1.020425574104004369E-16, 0.000000000000000000 ) ) ;
#7539 = DIRECTION ( 'NONE',  ( 0.000000000000000000, 0.000000000000000000, 1.000000000000000000 ) ) ;
#7540 = VECTOR ( 'NONE', #20912, 1000.000000000000000 ) ;
#7541 = CARTESIAN_POINT ( 'NONE',  ( -8.331955809010628045, 38.18181818181818699, -56.36098470834071605 ) ) ;
#7542 = AXIS2_PLACEMENT_3D ( 'NONE', #18449, #6419, #8248 ) ;
#7543 = ORIENTED_EDGE ( 'NONE', *, *, #17616, .T. ) ;
#7544 = DIRECTION ( 'NONE',  ( 0.000000000000000000, 0.000000000000000000, -1.000000000000000000 ) ) ;
#7545 = CARTESIAN_POINT ( 'NONE',  ( -0.7810292038144046600, 39.98537128388858264, -49.65442669227651606 ) ) ;
#7546 = DIRECTION ( 'NONE',  ( 6.505213034913038160E-19, 3.903127820947822896E-18, 1.000000000000000000 ) ) ;
#7547 = CARTESIAN_POINT ( 'NONE',  ( 9.852267639826706613, 8.683574217357186598, -43.21671877549182739 ) ) ;
#7548 = CIRCLE ( 'NONE', #21828, 19.11328065563152379 ) ;
#7549 = EDGE_LOOP ( 'NONE', ( #3169, #12624, #4885, #2974 ) ) ;
#7550 = EDGE_LOOP ( 'NONE', ( #8836, #5298 ) ) ;
#7551 = CARTESIAN_POINT ( 'NONE',  ( 7.310544252644470693E-15, 28.19616000222403684, 0.000000000000000000 ) ) ;
#7552 = DIRECTION ( 'NONE',  ( -6.505213034913038160E-19, -3.903127820947822896E-18, -1.000000000000000000 ) ) ;
#7553 = ORIENTED_EDGE ( 'NONE', *, *, #3537, .T. ) ;
#7554 = AXIS2_PLACEMENT_3D ( 'NONE', #12594, #10762, #15590 ) ;
#7555 = DIRECTION ( 'NONE',  ( -0.000000000000000000, -0.000000000000000000, -1.000000000000000000 ) ) ;
#7556 = DIRECTION ( 'NONE',  ( -0.000000000000000000, -1.000000000000000000, -0.000000000000000000 ) ) ;
#7557 = ORIENTED_EDGE ( 'NONE', *, *, #21057, .F. ) ;
#7558 = DIRECTION ( 'NONE',  ( -1.000000000000000000, 1.084202172485504434E-16, 0.000000000000000000 ) ) ;
#7559 = AXIS2_PLACEMENT_3D ( 'NONE', #19420, #12747, #610 ) ;
#7560 = DIRECTION ( 'NONE',  ( -6.505213034913038160E-19, -3.903127820947822896E-18, -1.000000000000000000 ) ) ;
#7561 = DIRECTION ( 'NONE',  ( 0.000000000000000000, 0.7071067811865507924, 0.7071067811865441310 ) ) ;
#7562 = ORIENTED_EDGE ( 'NONE', *, *, #17859, .F. ) ;
#7563 = FACE_BOUND ( 'NONE', #8195, .T. ) ;
#7564 = CARTESIAN_POINT ( 'NONE',  ( -8.640962819011734908, 40.00000000000000000, 53.20846273842203544 ) ) ;
#7565 = EDGE_LOOP ( 'NONE', ( #14703, #8828, #2530, #21570 ) ) ;
#7566 = DIRECTION ( 'NONE',  ( -0.000000000000000000, -0.000000000000000000, -1.000000000000000000 ) ) ;
#7567 = CYLINDRICAL_SURFACE ( 'NONE', #11988, 5.000000000000000000 ) ;
#7568 = CARTESIAN_POINT ( 'NONE',  ( 7.310544252644470693E-15, 28.19616000222403684, 0.000000000000000000 ) ) ;
#7569 = LINE ( 'NONE', #17650, #6291 ) ;
#7570 = EDGE_LOOP ( 'NONE', ( #7116, #20861, #6434, #8460 ) ) ;
#7571 = CARTESIAN_POINT ( 'NONE',  ( -36.75746821813305587, 0.6841746959067307454, 2.800654218530485018 ) ) ;
#7572 = DIRECTION ( 'NONE',  ( -0.4124789556921610312, -0.7071067811865332509, -0.5743353646704374427 ) ) ;
#7573 = CARTESIAN_POINT ( 'NONE',  ( -0.2316815189680993536, 39.99968400692258541, -48.91347655445596132 ) ) ;
#7574 = CIRCLE ( 'NONE', #241, 2.499999999999995115 ) ;
#7575 = EDGE_CURVE ( 'NONE', #14282, #18599, #10942, .T. ) ;
#7576 = ORIENTED_EDGE ( 'NONE', *, *, #12441, .F. ) ;
#7577 = CARTESIAN_POINT ( 'NONE',  ( -7.033428926742895548, 33.31269054942711705, 41.47353357286039710 ) ) ;
#7578 = CARTESIAN_POINT ( 'NONE',  ( 1.591932335265033587E-15, -4.923002280079127832E-27, 50.50395615645412306 ) ) ;
#7579 = ADVANCED_FACE ( 'NONE', ( #19439 ), #1593, .F. ) ;
#7580 = VERTEX_POINT ( 'NONE', #14602 ) ;
#7581 = VECTOR ( 'NONE', #5988, 1000.000000000000000 ) ;
#7582 = ORIENTED_EDGE ( 'NONE', *, *, #69, .F. ) ;
#7583 = VECTOR ( 'NONE', #21240, 1000.000000000000000 ) ;
#7584 = EDGE_LOOP ( 'NONE', ( #6312, #10404, #9483, #7831, #4540, #9189, #13316, #11715, #13750, #12289 ) ) ;
#7585 = AXIS2_PLACEMENT_3D ( 'NONE', #5021, #10925, #7273 ) ;
#7586 = ORIENTED_EDGE ( 'NONE', *, *, #6921, .T. ) ;
#7587 = DIRECTION ( 'NONE',  ( 0.000000000000000000, 0.000000000000000000, 1.000000000000000000 ) ) ;
#7588 = CARTESIAN_POINT ( 'NONE',  ( 0.000000000000000000, -45.00000000000000000, 0.000000000000000000 ) ) ;
#7589 = CARTESIAN_POINT ( 'NONE',  ( -21.00948735876882623, -24.79619811426206510, -6.999999999999950262 ) ) ;
#7590 = DIRECTION ( 'NONE',  ( 0.000000000000000000, 1.000000000000000000, 0.000000000000000000 ) ) ;
#7591 = EDGE_CURVE ( 'NONE', #18864, #575, #2238, .T. ) ;
#7592 = ORIENTED_EDGE ( 'NONE', *, *, #12367, .F. ) ;
#7593 = CARTESIAN_POINT ( 'NONE',  ( 12.24744603030438839, 40.00000000000000000, -54.43639671998947449 ) ) ;
#7594 = FACE_OUTER_BOUND ( 'NONE', #14440, .T. ) ;
#7595 = ORIENTED_EDGE ( 'NONE', *, *, #17800, .F. ) ;
#7596 = FACE_OUTER_BOUND ( 'NONE', #5100, .T. ) ;
#7597 = PLANE ( 'NONE',  #10097 ) ;
#7598 = DIRECTION ( 'NONE',  ( 6.505213034913038160E-19, 3.903127820947822896E-18, 1.000000000000000000 ) ) ;
#7599 = VERTEX_POINT ( 'NONE', #21488 ) ;
#7600 = CARTESIAN_POINT ( 'NONE',  ( 0.4211638912453626871, -0.02267170259972375174, 49.14966933622903156 ) ) ;
#7601 = AXIS2_PLACEMENT_3D ( 'NONE', #18464, #10083, #2780 ) ;
#7602 = EDGE_LOOP ( 'NONE', ( #7121, #15782 ) ) ;
#7603 = CARTESIAN_POINT ( 'NONE',  ( 2.775557561562891351E-14, -2.775557561562891351E-14, 2.999999999999999112 ) ) ;
#7604 = CONICAL_SURFACE ( 'NONE', #8693, 2.525000000000110489, 0.7853981633971014453 ) ;
#7605 = EDGE_CURVE ( 'NONE', #18834, #15969, #11470, .T. ) ;
#7606 = DIRECTION ( 'NONE',  ( 0.000000000000000000, -1.000000000000000000, 0.000000000000000000 ) ) ;
#7607 = EDGE_LOOP ( 'NONE', ( #4652, #5198, #2654, #714 ) ) ;
#7608 = DIRECTION ( 'NONE',  ( 0.000000000000000000, 0.000000000000000000, 1.000000000000000000 ) ) ;
#7609 = CIRCLE ( 'NONE', #6155, 2.499999999999998668 ) ;
#7610 = AXIS2_PLACEMENT_3D ( 'NONE', #3184, #4680, #11655 ) ;
#7611 = FACE_OUTER_BOUND ( 'NONE', #3258, .T. ) ;
#7612 = CARTESIAN_POINT ( 'NONE',  ( 25.58633464742632313, 23.74488952252767859, -2.999999999999971578 ) ) ;
#7613 = EDGE_CURVE ( 'NONE', #6403, #13845, #417, .T. ) ;
#7614 = DIRECTION ( 'NONE',  ( 1.000000000000000000, 0.000000000000000000, 0.000000000000000000 ) ) ;
#7615 = ORIENTED_EDGE ( 'NONE', *, *, #14210, .F. ) ;
#7616 = EDGE_LOOP ( 'NONE', ( #1623, #20928, #495, #1635 ) ) ;
#7617 = CONICAL_SURFACE ( 'NONE', #21887, 49.99999999999998579, 0.7853981633974691512 ) ;
#7618 = ORIENTED_EDGE ( 'NONE', *, *, #18490, .F. ) ;
#7619 = EDGE_LOOP ( 'NONE', ( #17672, #12687, #15073, #21703 ) ) ;
#7620 = DIRECTION ( 'NONE',  ( -0.000000000000000000, 1.000000000000000000, -0.000000000000000000 ) ) ;
#7621 = CIRCLE ( 'NONE', #706, 19.11328065563151668 ) ;
#7622 = CARTESIAN_POINT ( 'NONE',  ( 14.93538271375424742, 34.13396246814581758, -7.000000000000006217 ) ) ;
#7623 = CIRCLE ( 'NONE', #5807, 31.50000000000000711 ) ;
#7624 = CARTESIAN_POINT ( 'NONE',  ( 5.999999999999999112, -40.00000000000000000, -6.000000000000000000 ) ) ;
#7625 = EDGE_CURVE ( 'NONE', #21079, #15231, #13272, .T. ) ;
#7626 = AXIS2_PLACEMENT_3D ( 'NONE', #3980, #9229, #21272 ) ;
#7627 = ORIENTED_EDGE ( 'NONE', *, *, #14322, .F. ) ;
#7628 = CARTESIAN_POINT ( 'NONE',  ( -9.689843208404433028, 39.33333333333334991, -54.54983754392741702 ) ) ;
#7629 = DIRECTION ( 'NONE',  ( -1.000000000000000000, 0.000000000000000000, 0.000000000000000000 ) ) ;
#7630 = CIRCLE ( 'NONE', #10162, 41.00000000000000000 ) ;
#7631 = ORIENTED_EDGE ( 'NONE', *, *, #15790, .T. ) ;
#7632 = LINE ( 'NONE', #14938, #21446 ) ;
#7633 = FACE_OUTER_BOUND ( 'NONE', #22221, .T. ) ;
#7634 = EDGE_CURVE ( 'NONE', #7992, #2079, #10012, .T. ) ;
#7635 = CARTESIAN_POINT ( 'NONE',  ( 15.62726112422616076, 28.45046755804886374, -2.999999999999971578 ) ) ;
#7636 = EDGE_CURVE ( 'NONE', #6902, #20227, #7394, .T. ) ;
#7637 = DIRECTION ( 'NONE',  ( -1.000000000000000000, 0.000000000000000000, 0.000000000000000000 ) ) ;
#7638 = DIRECTION ( 'NONE',  ( 0.000000000000000000, 0.000000000000000000, -1.000000000000000000 ) ) ;
#7639 = AXIS2_PLACEMENT_3D ( 'NONE', #17540, #7005, #3236 ) ;
#7640 = AXIS2_PLACEMENT_3D ( 'NONE', #225, #14536, #5388 ) ;
#7641 = AXIS2_PLACEMENT_3D ( 'NONE', #18480, #18601, #9611 ) ;
#7642 = CARTESIAN_POINT ( 'NONE',  ( -30.57187188083506157, -7.711478842616581453, -2.999999999999971578 ) ) ;
#7643 = DIRECTION ( 'NONE',  ( 6.505213034913038160E-19, 3.903127820947822896E-18, 1.000000000000000000 ) ) ;
#7644 = EDGE_CURVE ( 'NONE', #7232, #17346, #7286, .T. ) ;
#7645 = VERTEX_POINT ( 'NONE', #5555 ) ;
#7646 = VERTEX_POINT ( 'NONE', #12533 ) ;
#7647 = EDGE_CURVE ( 'NONE', #8904, #15024, #9917, .T. ) ;
#7648 = ORIENTED_EDGE ( 'NONE', *, *, #18549, .F. ) ;
#7649 = CARTESIAN_POINT ( 'NONE',  ( 1.110223024625156540E-13, -5.551115123125782702E-14, -6.999999999999950262 ) ) ;
#7650 = EDGE_CURVE ( 'NONE', #15602, #22642, #19061, .T. ) ;
#7651 = AXIS2_PLACEMENT_3D ( 'NONE', #21236, #12404, #8966 ) ;
#7652 = CYLINDRICAL_SURFACE ( 'NONE', #2116, 60.00000000000000000 ) ;
#7653 = CARTESIAN_POINT ( 'NONE',  ( -0.05288783471925459501, -1.234056376215191486, -48.20419181041116019 ) ) ;
#7654 = CARTESIAN_POINT ( 'NONE',  ( 1.007402651613724608E-12, -1.880345380268765651E-13, 50.27953280580743467 ) ) ;
#7655 = CARTESIAN_POINT ( 'NONE',  ( -19.60425726290410964, 16.02072691545761174, 60.52684394361300235 ) ) ;
#7656 = CARTESIAN_POINT ( 'NONE',  ( -1.510243460696181139E-14, 40.00000000000000000, -48.73397172404481381 ) ) ;
#7657 = ORIENTED_EDGE ( 'NONE', *, *, #18367, .F. ) ;
#7658 = DIRECTION ( 'NONE',  ( 0.000000000000000000, 0.000000000000000000, -1.000000000000000000 ) ) ;
#7659 = CYLINDRICAL_SURFACE ( 'NONE', #2084, 15.00000000000000000 ) ;
#7660 = ORIENTED_EDGE ( 'NONE', *, *, #17157, .F. ) ;
#7661 = CARTESIAN_POINT ( 'NONE',  ( 12.00937115242650677, 34.74700806321084912, -1.999999999999977573 ) ) ;
#7662 = CARTESIAN_POINT ( 'NONE',  ( 4.025500340002707844, -36.54278193890314697, -2.800654218530457484 ) ) ;
#7663 = DIRECTION ( 'NONE',  ( 0.000000000000000000, 0.000000000000000000, 1.000000000000000000 ) ) ;
#7664 = EDGE_CURVE ( 'NONE', #20382, #7125, #18331, .T. ) ;
#7665 = ORIENTED_EDGE ( 'NONE', *, *, #17045, .T. ) ;
#7666 = FACE_BOUND ( 'NONE', #9885, .T. ) ;
#7667 = ORIENTED_EDGE ( 'NONE', *, *, #7591, .F. ) ;
#7668 = PRESENTATION_LAYER_ASSIGNMENT (  '', '', ( #15333 ) ) ;
#7669 = CARTESIAN_POINT ( 'NONE',  ( -37.07861450834822392, 3.656418565264024423, 2.999999999999995559 ) ) ;
#7670 = CARTESIAN_POINT ( 'NONE',  ( 35.00000000000058265, 40.00000000000000000, -52.50000000000076739 ) ) ;
#7671 = ORIENTED_EDGE ( 'NONE', *, *, #18661, .F. ) ;
#7672 = DIRECTION ( 'NONE',  ( 6.505213034913038160E-19, 3.903127820947822896E-18, 1.000000000000000000 ) ) ;
#7673 = CARTESIAN_POINT ( 'NONE',  ( -4.170748987303213084, 34.65667543218822999, -2.999999999999971578 ) ) ;
#7674 = EDGE_LOOP ( 'NONE', ( #18467, #8840 ) ) ;
#7675 = FACE_OUTER_BOUND ( 'NONE', #3601, .T. ) ;
#7676 = AXIS2_PLACEMENT_3D ( 'NONE', #4903, #18878, #8119 ) ;
#7677 = CYLINDRICAL_SURFACE ( 'NONE', #3256, 1.000000000000000888 ) ;
#7678 = ORIENTED_EDGE ( 'NONE', *, *, #5597, .F. ) ;
#7679 = FACE_OUTER_BOUND ( 'NONE', #14124, .T. ) ;
#7680 = CARTESIAN_POINT ( 'NONE',  ( -12.84005703549979849, 1.693876179609747012, -55.76322220629404569 ) ) ;
#7681 = EDGE_LOOP ( 'NONE', ( #9596, #20791, #6503, #4051 ) ) ;
#7682 = CARTESIAN_POINT ( 'NONE',  ( -34.99999999999999289, 5.000000000000000000, 9.999999999999971578 ) ) ;
#7683 = CARTESIAN_POINT ( 'NONE',  ( 11.86180952234342278, 38.99999999999291589, -55.35904751185374550 ) ) ;
#7684 = DIRECTION ( 'NONE',  ( 6.505213034913038160E-19, 3.903127820947822896E-18, 1.000000000000000000 ) ) ;
#7685 = ORIENTED_EDGE ( 'NONE', *, *, #13301, .T. ) ;
#7686 = DIRECTION ( 'NONE',  ( 0.000000000000000000, 0.000000000000000000, -1.000000000000000000 ) ) ;
#7687 = FACE_BOUND ( 'NONE', #1899, .T. ) ;
#7688 = FACE_OUTER_BOUND ( 'NONE', #12227, .T. ) ;
#7689 = ADVANCED_FACE ( 'NONE', ( #5793, #12768 ), #19779, .F. ) ;
#7690 = ORIENTED_EDGE ( 'NONE', *, *, #12524, .T. ) ;
#7691 = CARTESIAN_POINT ( 'NONE',  ( -34.99999999999980815, 28.00000000000000000, 57.09999999999921982 ) ) ;
#7692 = CIRCLE ( 'NONE', #13526, 59.99999999999703704 ) ;
#7693 = CARTESIAN_POINT ( 'NONE',  ( -13.76792553423404186, 26.00189441538239876, 45.26963775109940968 ) ) ;
#7694 = LINE ( 'NONE', #21673, #3780 ) ;
#7695 = AXIS2_PLACEMENT_3D ( 'NONE', #12736, #12956, #16407 ) ;
#7696 = ADVANCED_FACE ( 'NONE', ( #20456 ), #2587, .F. ) ;
#7697 = ORIENTED_EDGE ( 'NONE', *, *, #527, .F. ) ;
#7698 = ORIENTED_EDGE ( 'NONE', *, *, #7997, .T. ) ;
#7699 = ORIENTED_EDGE ( 'NONE', *, *, #7908, .F. ) ;
#7700 = EDGE_CURVE ( 'NONE', #18105, #22110, #8098, .T. ) ;
#7701 = VERTEX_POINT ( 'NONE', #856 ) ;
#7702 = DIRECTION ( 'NONE',  ( -6.505213034913038160E-19, -3.903127820947822896E-18, -1.000000000000000000 ) ) ;
#7703 = CIRCLE ( 'NONE', #6242, 19.11328065563152379 ) ;
#7704 = CARTESIAN_POINT ( 'NONE',  ( 35.00000000000000000, -5.000000000000000000, 54.99999999999698019 ) ) ;
#7705 = CARTESIAN_POINT ( 'NONE',  ( -31.92986134326219982, 18.22261011550282817, -2.800654218530485018 ) ) ;
#7706 = LINE ( 'NONE', #9539, #10530 ) ;
#7707 = VERTEX_POINT ( 'NONE', #21956 ) ;
#7708 = DIRECTION ( 'NONE',  ( -6.505213034913038160E-19, -3.903127820947822896E-18, -1.000000000000000000 ) ) ;
#7709 = CARTESIAN_POINT ( 'NONE',  ( -42.49999999999996447, 10.00000000000000000, -47.50000000000000711 ) ) ;
#7710 = ORIENTED_EDGE ( 'NONE', *, *, #10953, .F. ) ;
#7711 = PLANE ( 'NONE',  #19671 ) ;
#7712 = CARTESIAN_POINT ( 'NONE',  ( -19.90501858586609174, 9.588439829449736607, -58.07150046051949488 ) ) ;
#7713 = EDGE_CURVE ( 'NONE', #8041, #22419, #6247, .T. ) ;
#7714 = CARTESIAN_POINT ( 'NONE',  ( 15.61498135782973584, 7.478867266539133141, -59.38575377909876352 ) ) ;
#7715 = ORIENTED_EDGE ( 'NONE', *, *, #10073, .T. ) ;
#7716 = CARTESIAN_POINT ( 'NONE',  ( -9.103081159019540181, 0.03030367950604016467, 53.87333532811888404 ) ) ;
#7717 = LINE ( 'NONE', #2569, #12366 ) ;
#7718 = ORIENTED_EDGE ( 'NONE', *, *, #19289, .F. ) ;
#7719 = CARTESIAN_POINT ( 'NONE',  ( 5.617739682035653992, 39.81210785744588065, 52.56498351368300348 ) ) ;
#7720 = DIRECTION ( 'NONE',  ( 1.000000000000000000, 0.000000000000000000, 0.000000000000000000 ) ) ;
#7721 = ORIENTED_EDGE ( 'NONE', *, *, #4187, .F. ) ;
#7722 = CARTESIAN_POINT ( 'NONE',  ( 16.99999999999997513, 20.00000000000000355, 102.0000000000000142 ) ) ;
#7723 = CARTESIAN_POINT ( 'NONE',  ( 15.24242605747179802, 36.49796895611718384, 56.65858500684291243 ) ) ;
#7724 = CARTESIAN_POINT ( 'NONE',  ( -31.09841355225981374, 5.093313992686310243, -7.000000000000006217 ) ) ;
#7725 = CIRCLE ( 'NONE', #20525, 19.99999999999999289 ) ;
#7726 = VECTOR ( 'NONE', #138, 1000.000000000000000 ) ;
#7727 = CARTESIAN_POINT ( 'NONE',  ( 11.24990497771462827, 36.62343892044964377, -57.74518096503230424 ) ) ;
#7728 = ORIENTED_EDGE ( 'NONE', *, *, #12745, .T. ) ;
#7729 = ORIENTED_EDGE ( 'NONE', *, *, #17140, .T. ) ;
#7730 = EDGE_LOOP ( 'NONE', ( #22023, #20304, #9905, #4329 ) ) ;
#7731 = EDGE_CURVE ( 'NONE', #11090, #18872, #20562, .T. ) ;
#7732 = EDGE_LOOP ( 'NONE', ( #21914, #13397, #15186, #1406 ) ) ;
#7733 = FACE_OUTER_BOUND ( 'NONE', #7359, .T. ) ;
#7734 = DIRECTION ( 'NONE',  ( 1.296372316667914327E-16, 1.000000000000000000, -0.000000000000000000 ) ) ;
#7735 = AXIS2_PLACEMENT_3D ( 'NONE', #7996, #4786, #4558 ) ;
#7736 = CARTESIAN_POINT ( 'NONE',  ( -15.02862401740788556, -32.75570538720795355, 3.000000000000002665 ) ) ;
#7737 = ORIENTED_EDGE ( 'NONE', *, *, #7049, .F. ) ;
#7738 = DIRECTION ( 'NONE',  ( 1.000000000000000000, 0.000000000000000000, 0.000000000000000000 ) ) ;
#7739 = DIRECTION ( 'NONE',  ( -6.505213034913038160E-19, -3.903127820947822896E-18, -1.000000000000000000 ) ) ;
#7740 = EDGE_CURVE ( 'NONE', #10900, #3760, #4432, .T. ) ;
#7741 = ADVANCED_BREP_SHAPE_REPRESENTATION ( '', ( #17721, #18273 ), #10192 ) ;
#7742 = ORIENTED_EDGE ( 'NONE', *, *, #13596, .T. ) ;
#7743 = DIRECTION ( 'NONE',  ( -1.000000000000000000, -1.208970125616081209E-17, 0.000000000000000000 ) ) ;
#7744 = CARTESIAN_POINT ( 'NONE',  ( 17.86915608785696818, -27.01645732367869002, -2.999999999999971578 ) ) ;
#7745 = CARTESIAN_POINT ( 'NONE',  ( 29.33526866242100439, -22.15900668633777215, -2.800654218530429507 ) ) ;
#7746 = DIRECTION ( 'NONE',  ( -6.505213034913038160E-19, -3.903127820947822896E-18, -1.000000000000000000 ) ) ;
#7747 = CIRCLE ( 'NONE', #11393, 31.50000000000000000 ) ;
#7748 = DIRECTION ( 'NONE',  ( -1.000000000000000000, 0.000000000000000000, 0.000000000000000000 ) ) ;
#7749 = EDGE_CURVE ( 'NONE', #16771, #7803, #12104, .T. ) ;
#7750 = FACE_OUTER_BOUND ( 'NONE', #11665, .T. ) ;
#7751 = ORIENTED_EDGE ( 'NONE', *, *, #9752, .T. ) ;
#7752 = ORIENTED_EDGE ( 'NONE', *, *, #16173, .T. ) ;
#7753 = EDGE_CURVE ( 'NONE', #13978, #7988, #2973, .T. ) ;
#7754 = ORIENTED_EDGE ( 'NONE', *, *, #15877, .T. ) ;
#7755 = DIRECTION ( 'NONE',  ( 1.000000000000000000, -1.084202172485504927E-16, 0.000000000000000000 ) ) ;
#7756 = DIRECTION ( 'NONE',  ( 1.296372316667914327E-16, 1.000000000000000000, -0.000000000000000000 ) ) ;
#7757 = B_SPLINE_CURVE_WITH_KNOTS ( 'NONE', 3,
 ( #10792, #12188, #5321, #7033 ),
 .UNSPECIFIED., .F., .F.,
 ( 4, 4 ),
 ( 0.001875451646902607204, 0.003761979286331133213 ),
 .UNSPECIFIED. ) ;
#7758 = CIRCLE ( 'NONE', #16153, 4.025000000000000355 ) ;
#7759 = DIRECTION ( 'NONE',  ( 1.000000000000000000, 0.000000000000000000, -0.000000000000000000 ) ) ;
#7760 = CARTESIAN_POINT ( 'NONE',  ( 19.99999999999998579, 20.00000000000000711, -60.62177826491069510 ) ) ;
#7761 = CARTESIAN_POINT ( 'NONE',  ( -6.869624750922561418, 39.72564401595366945, -53.24680511806212024 ) ) ;
#7762 = DIRECTION ( 'NONE',  ( -6.505213034913038160E-19, -3.903127820947822896E-18, -1.000000000000000000 ) ) ;
#7763 = CARTESIAN_POINT ( 'NONE',  ( 35.00000000000058265, 40.00000000000000711, -55.00000000000076028 ) ) ;
#7764 = ORIENTED_EDGE ( 'NONE', *, *, #9254, .T. ) ;
#7765 = CARTESIAN_POINT ( 'NONE',  ( -34.24928931925748543, 6.742883674876520850, -2.999999999999957367 ) ) ;
#7766 = DIRECTION ( 'NONE',  ( 6.505213034913038160E-19, 3.903127820947822896E-18, 1.000000000000000000 ) ) ;
#7767 = CARTESIAN_POINT ( 'NONE',  ( 4.898587196589408884E-16, 30.00000000000000000, -3.999999999999996447 ) ) ;
#7768 = ORIENTED_EDGE ( 'NONE', *, *, #12181, .F. ) ;
#7769 = EDGE_LOOP ( 'NONE', ( #22136, #9696, #18929, #7665, #11529, #18252 ) ) ;
#7770 = EDGE_CURVE ( 'NONE', #1187, #2480, #15757, .T. ) ;
#7771 = DIRECTION ( 'NONE',  ( 6.505213034913038160E-19, 3.903127820947822896E-18, 1.000000000000000000 ) ) ;
#7772 = DIRECTION ( 'NONE',  ( -6.505213034913038160E-19, -3.903127820947822896E-18, -1.000000000000000000 ) ) ;
#7773 = AXIS2_PLACEMENT_3D ( 'NONE', #20396, #20284, #4473 ) ;
#7774 = AXIS2_PLACEMENT_3D ( 'NONE', #4762, #10003, #16995 ) ;
#7775 = EDGE_CURVE ( 'NONE', #2030, #9978, #4867, .T. ) ;
#7776 = EDGE_CURVE ( 'NONE', #15580, #11720, #18697, .T. ) ;
#7777 = EDGE_LOOP ( 'NONE', ( #13651, #6267, #20305, #12890 ) ) ;
#7778 = VECTOR ( 'NONE', #14237, 1000.000000000000000 ) ;
#7779 = ADVANCED_FACE ( 'NONE', ( #10116 ), #17336, .F. ) ;
#7780 = CARTESIAN_POINT ( 'NONE',  ( -17.38064605515553041, -30.98879172160219042, 3.000000000000063505 ) ) ;
#7781 = CARTESIAN_POINT ( 'NONE',  ( 7.531932117834364782, 39.99999999999999289, -52.77310570466495676 ) ) ;
#7782 = ORIENTED_EDGE ( 'NONE', *, *, #16769, .T. ) ;
#7783 = CARTESIAN_POINT ( 'NONE',  ( 2.669015549682804078, 39.95797184809391212, -50.69824233904017063 ) ) ;
#7784 = LINE ( 'NONE', #11449, #11713 ) ;
#7785 = ADVANCED_FACE ( 'NONE', ( #8414 ), #22636, .F. ) ;
#7786 = VERTEX_POINT ( 'NONE', #3607 ) ;
#7787 = LINE ( 'NONE', #4246, #4495 ) ;
#7788 = CARTESIAN_POINT ( 'NONE',  ( 10.50000000000024514, -2.516660498395250745, -105.0000000000000142 ) ) ;
#7789 = DIRECTION ( 'NONE',  ( 0.000000000000000000, 0.000000000000000000, -1.000000000000000000 ) ) ;
#7790 = CARTESIAN_POINT ( 'NONE',  ( 3.330669073875469621E-13, -1.110223024625156540E-13, -2.999999999999971578 ) ) ;
#7791 = AXIS2_PLACEMENT_3D ( 'NONE', #11417, #20367, #7994 ) ;
#7792 = CYLINDRICAL_SURFACE ( 'NONE', #17635, 2.099999999999997868 ) ;
#7793 = ORIENTED_EDGE ( 'NONE', *, *, #21182, .T. ) ;
#7794 = DIRECTION ( 'NONE',  ( 0.000000000000000000, 0.000000000000000000, 1.000000000000000000 ) ) ;
#7795 = CARTESIAN_POINT ( 'NONE',  ( 24.62019382530528233, -4.341204441673129466, 3.000000000000023537 ) ) ;
#7796 = DIRECTION ( 'NONE',  ( 0.000000000000000000, 0.000000000000000000, -1.000000000000000000 ) ) ;
#7797 = ORIENTED_EDGE ( 'NONE', *, *, #11966, .T. ) ;
#7798 = DIRECTION ( 'NONE',  ( 0.000000000000000000, 0.000000000000000000, -1.000000000000000000 ) ) ;
#7799 = DIRECTION ( 'NONE',  ( -0.8391477167891884248, 0.3845457931435832810, -0.3846500258456567733 ) ) ;
#7800 = CARTESIAN_POINT ( 'NONE',  ( -33.47097213929426829, 11.93830856187182832, 3.000000000000058620 ) ) ;
#7801 = ORIENTED_EDGE ( 'NONE', *, *, #15860, .F. ) ;
#7802 = CIRCLE ( 'NONE', #3072, 17.00000000000000000 ) ;
#7803 = VERTEX_POINT ( 'NONE', #3490 ) ;
#7804 = AXIS2_PLACEMENT_3D ( 'NONE', #13604, #3096, #10066 ) ;
#7805 = CARTESIAN_POINT ( 'NONE',  ( 188.2704906108920113, 176.3972761393069106, 8.483359203117380787 ) ) ;
#7806 = UNCERTAINTY_MEASURE_WITH_UNIT (LENGTH_MEASURE( 1.000000000000000082E-05 ), #12569, 'distance_accuracy_value', 'NONE');
#7807 = AXIS2_PLACEMENT_3D ( 'NONE', #7923, #14883, #11583 ) ;
#7808 = ADVANCED_FACE ( 'NONE', ( #17224, #20904 ), #13774, .F. ) ;
#7809 = ORIENTED_EDGE ( 'NONE', *, *, #18522, .T. ) ;
#7810 = CARTESIAN_POINT ( 'NONE',  ( 10.79056263833815343, 40.00000000000000711, 53.90082266129228117 ) ) ;
#7811 = CARTESIAN_POINT ( 'NONE',  ( 5.961618526222387082, -3.061744126944893729, 51.29856354178728850 ) ) ;
#7812 = CARTESIAN_POINT ( 'NONE',  ( 35.00000000000000000, 10.00000000000000000, -40.99999999999997868 ) ) ;
#7813 = EDGE_CURVE ( 'NONE', #16292, #4303, #22402, .T. ) ;
#7814 = CARTESIAN_POINT ( 'NONE',  ( -42.50000000000000711, -9.600000000000001421, 45.40000000000001279 ) ) ;
#7815 = CARTESIAN_POINT ( 'NONE',  ( 89.99999999999701572, -5.000000000000000000, -2.500000000000060840 ) ) ;
#7816 = VERTEX_POINT ( 'NONE', #3267 ) ;
#7817 = DIRECTION ( 'NONE',  ( 0.000000000000000000, 0.000000000000000000, -1.000000000000000000 ) ) ;
#7818 = LINE ( 'NONE', #4619, #13422 ) ;
#7819 = ORIENTED_EDGE ( 'NONE', *, *, #6487, .F. ) ;
#7820 = CARTESIAN_POINT ( 'NONE',  ( -15.00000000000001421, 20.00000000000000355, 101.0000000000000568 ) ) ;
#7821 = CARTESIAN_POINT ( 'NONE',  ( -90.00000000000000000, 40.00000000000000000, -9.108981535246192915E-16 ) ) ;
#7822 = VECTOR ( 'NONE', #157, 1000.000000000000000 ) ;
#7823 = DIRECTION ( 'NONE',  ( 1.000000000000000000, 0.000000000000000000, 0.000000000000000000 ) ) ;
#7824 = ORIENTED_EDGE ( 'NONE', *, *, #20103, .F. ) ;
#7825 = CARTESIAN_POINT ( 'NONE',  ( 36.14481870267517394, -0.8626474017862676424, 2.932969818539060469 ) ) ;
#7826 = CARTESIAN_POINT ( 'NONE',  ( -1.045703040280250073, 0.02735608008922960077, 49.70561346074470777 ) ) ;
#7827 = ADVANCED_FACE ( 'NONE', ( #17565 ), #1592, .T. ) ;
#7828 = ORIENTED_EDGE ( 'NONE', *, *, #1550, .F. ) ;
#7829 = CARTESIAN_POINT ( 'NONE',  ( 1.427805587809481747, 39.96253296377607001, 50.08434700428703223 ) ) ;
#7830 = CARTESIAN_POINT ( 'NONE',  ( -2.517789369293989221, 0.1458720723281411724, -52.33403986263111562 ) ) ;
#7831 = ORIENTED_EDGE ( 'NONE', *, *, #13981, .T. ) ;
#7832 = VECTOR ( 'NONE', #2403, 1000.000000000000000 ) ;
#7833 = CARTESIAN_POINT ( 'NONE',  ( 9.081037608041055975, 37.83854577724110868, 56.73868670301713024 ) ) ;
#7834 = LINE ( 'NONE', #8290, #21693 ) ;
#7835 = VECTOR ( 'NONE', #14740, 1000.000000000000000 ) ;
#7836 = AXIS2_PLACEMENT_3D ( 'NONE', #3094, #1718, #22354 ) ;
#7837 = CARTESIAN_POINT ( 'NONE',  ( -8.256135806682758371, -0.3920627093389252860, -55.63523492904088386 ) ) ;
#7838 = ORIENTED_EDGE ( 'NONE', *, *, #13992, .T. ) ;
#7839 = EDGE_CURVE ( 'NONE', #12263, #3967, #17906, .T. ) ;
#7840 = EDGE_LOOP ( 'NONE', ( #20556, #20387, #12528, #17656, #10909, #22302 ) ) ;
#7841 = CIRCLE ( 'NONE', #3473, 2.499999999999996891 ) ;
#7842 = EDGE_LOOP ( 'NONE', ( #2150, #21603, #14880, #18396 ) ) ;
#7843 = ORIENTED_EDGE ( 'NONE', *, *, #777, .F. ) ;
#7844 = CARTESIAN_POINT ( 'NONE',  ( 9.689843208404433028, 39.33333333333334991, 54.54983754392749518 ) ) ;
#7845 = CIRCLE ( 'NONE', #20655, 2.499999999999995115 ) ;
#7846 = CARTESIAN_POINT ( 'NONE',  ( 2.999999999999997780, 30.00000000000000000, 8.485281374238567764 ) ) ;
#7847 = EDGE_LOOP ( 'NONE', ( #14655, #5971, #8418, #10855 ) ) ;
#7848 = DIRECTION ( 'NONE',  ( -0.000000000000000000, 1.000000000000000000, -0.000000000000000000 ) ) ;
#7849 = CARTESIAN_POINT ( 'NONE',  ( -14.14132741310364416, -16.85297774861788156, -2.999999999999988898 ) ) ;
#7850 = EDGE_LOOP ( 'NONE', ( #17060, #8517, #16089, #4134 ) ) ;
#7851=STYLED_ITEM('',(#22741),#10851);
#7852 = ORIENTED_EDGE ( 'NONE', *, *, #5933, .F. ) ;
#7853 = DIRECTION ( 'NONE',  ( 6.505213034913038160E-19, 3.903127820947822896E-18, 1.000000000000000000 ) ) ;
#7854 = DIRECTION ( 'NONE',  ( -0.000000000000000000, -0.000000000000000000, -1.000000000000000000 ) ) ;
#7855 = DIRECTION ( 'NONE',  ( 0.000000000000000000, -1.000000000000000000, 0.000000000000000000 ) ) ;
#7856 = DIRECTION ( 'NONE',  ( -6.505213034913038160E-19, -3.903127820947822896E-18, -1.000000000000000000 ) ) ;
#7857 = CLOSED_SHELL ( 'NONE', ( #8203, #6163, #966, #393, #6822, #15547, #12627, #10306, #7280, #20246, #15451, #14457, #19407, #8857, #17278, #15654, #12090, #12648, #4098, #6248, #9308, #1966, #18774, #22457, #11594, #19145, #8318, #15152, #5898, #13096, #17902, #17469, #2284, #11705, #1107, #4323, #15743, #13804, #11878, #19239, #1031, #19957, #14903, #1943, #1443, #15197, #5627, #15832, #20117, #6517, #12052, #14238, #16820, #14351, #9178, #19778, #62, #5091, #15380, #9307, #20319, #13835, #11915, #16938, #914, #1640, #3735, #21114, #2461, #21479, #11975, #1210, #11139, #1599, #21471, #16125, #1758, #10295, #10150, #7785, #11110, #9916, #2828, #13541, #2172, #21788, #8169, #7496, #15190, #20955, #11173, #6296, #4805, #1690, #19668, #16103, #21918, #7417, #208, #13353, #20112, #18655, #6386, #15286, #10791, #12940, #5031, #757, #18670, #20778, #14037, #8235, #11306, #20950, #17864, #1479, #15007, #22669, #1587, #19480, #3125, #14505, #3804, #879, #4721, #7989, #16919, #13493, #14830, #17435, #679, #2153, #8343, #3330, #6019, #12842, #16219, #134, #4240, #15605, #9965, #8673, #20013, #11292, #22297, #20295, #21871, #20108, #11752, #1532, #20069, #12732, #4141, #21377, #11851, #6423, #11315, #11179, #2251, #4911, #11428, #7689, #4021, #22351, #6917, #2325, #17181, #17097, #987, #20584, #10139, #16134, #18833, #10595, #4361, #2773, #15850, #13170, #14327, #14980, #6569, #26, #6886, #11236, #18196, #11087, #17714, #4813, #20967, #10673, #10582, #2999, #5559, #20297, #223, #21658, #7779, #4722, #21224, #21774, #18103, #18122, #4978, #5282, #6661, #6518, #12396, #4518, #20337, #9621, #776, #9572, #15793, #5541, #4601, #10931, #20489, #16174, #19268, #311, #6213, #1433, #8881, #10384, #20554, #5134, #14057, #15645, #12718, #12125, #71, #769, #7827, #15028, #12517, #8456, #13640, #17423, #5538, #2922, #2495, #1004, #391, #22563, #1572, #12437 ) ) ;
#7858 = B_SPLINE_CURVE_WITH_KNOTS ( 'NONE', 3,
 ( #16554, #18382, #1307, #2701 ),
 .UNSPECIFIED., .F., .F.,
 ( 4, 4 ),
 ( 0.001893031756885266799, 0.003808480026563702565 ),
 .UNSPECIFIED. ) ;
#7859 = EDGE_CURVE ( 'NONE', #3604, #11652, #11746, .T. ) ;
#7860 = LINE ( 'NONE', #6149, #2863 ) ;
#7861 = CIRCLE ( 'NONE', #541, 0.9999999999999974465 ) ;
#7862 = CARTESIAN_POINT ( 'NONE',  ( -1.265314100866710527E-14, 40.00000000000000000, 48.73397172404484223 ) ) ;
#7863 = DIRECTION ( 'NONE',  ( 6.505213034913038160E-19, 3.903127820947822896E-18, 1.000000000000000000 ) ) ;
#7864 = ORIENTED_EDGE ( 'NONE', *, *, #22665, .F. ) ;
#7865 = EDGE_CURVE ( 'NONE', #18519, #15720, #480, .T. ) ;
#7866 = EDGE_CURVE ( 'NONE', #19753, #18815, #16826, .T. ) ;
#7867 = EDGE_LOOP ( 'NONE', ( #22555, #12606, #11017, #754 ) ) ;
#7868 = VECTOR ( 'NONE', #18660, 1000.000000000000000 ) ;
#7869 = EDGE_LOOP ( 'NONE', ( #16019, #4656 ) ) ;
#7870 = CARTESIAN_POINT ( 'NONE',  ( -19.48215071169293111, 15.15508441933061334, 58.00945324420519000 ) ) ;
#7871 = DIRECTION ( 'NONE',  ( -1.296372316667914327E-16, -1.000000000000000000, 0.000000000000000000 ) ) ;
#7872 = AXIS2_PLACEMENT_3D ( 'NONE', #4662, #6598, #13562 ) ;
#7873 = CYLINDRICAL_SURFACE ( 'NONE', #18950, 2.500000000000008882 ) ;
#7874 = CARTESIAN_POINT ( 'NONE',  ( 7.545596340824617165, -0.4932457138987723644, -52.99914579202174281 ) ) ;
#7875 = AXIS2_PLACEMENT_3D ( 'NONE', #6784, #14080, #1626 ) ;
#7876 = CARTESIAN_POINT ( 'NONE',  ( 12.31876324338296236, 30.07487443287962137, -6.999999999999950262 ) ) ;
#7877 = ADVANCED_FACE ( 'NONE', ( #9086 ), #6626, .T. ) ;
#7878 = DIRECTION ( 'NONE',  ( 0.000000000000000000, 0.000000000000000000, 1.000000000000000000 ) ) ;
#7879 = CYLINDRICAL_SURFACE ( 'NONE', #5088, 17.00000000000000000 ) ;
#7880 = DIRECTION ( 'NONE',  ( 6.505213034913038160E-19, 3.903127820947822896E-18, 1.000000000000000000 ) ) ;
#7881 = CARTESIAN_POINT ( 'NONE',  ( -10.39230484541309174, -25.00000000000000000, 5.999999999999708677 ) ) ;
#7882 = FACE_OUTER_BOUND ( 'NONE', #13438, .T. ) ;
#7883 = CARTESIAN_POINT ( 'NONE',  ( -33.99999999999998579, 28.19616000222404040, 0.000000000000000000 ) ) ;
#7884 = ORIENTED_EDGE ( 'NONE', *, *, #5380, .F. ) ;
#7885 = DIRECTION ( 'NONE',  ( 6.505213034913038160E-19, 3.903127820947822896E-18, 1.000000000000000000 ) ) ;
#7886 = DIRECTION ( 'NONE',  ( -6.505213034913038160E-19, -3.903127820947822896E-18, -1.000000000000000000 ) ) ;
#7887 = CYLINDRICAL_SURFACE ( 'NONE', #17900, 3.000000000000002665 ) ;
#7888 = CARTESIAN_POINT ( 'NONE',  ( 12.27586057105636108, 4.193657236093906171, 55.54740530680977884 ) ) ;
#7889 = EDGE_CURVE ( 'NONE', #9501, #790, #14659, .T. ) ;
#7890 = LINE ( 'NONE', #20040, #18802 ) ;
#7891 = ORIENTED_EDGE ( 'NONE', *, *, #20702, .F. ) ;
#7892 = AXIS2_PLACEMENT_3D ( 'NONE', #7790, #4476, #16146 ) ;
#7893 = ORIENTED_EDGE ( 'NONE', *, *, #11989, .T. ) ;
#7894 = DIRECTION ( 'NONE',  ( 0.000000000000000000, 0.000000000000000000, 1.000000000000000000 ) ) ;
#7895 = CARTESIAN_POINT ( 'NONE',  ( 42.49999999999998579, 10.00000000000000000, -47.49999999999997868 ) ) ;
#7896 = VECTOR ( 'NONE', #11080, 1000.000000000000000 ) ;
#7897 = EDGE_CURVE ( 'NONE', #4746, #21718, #18009, .T. ) ;
#7898 = AXIS2_PLACEMENT_3D ( 'NONE', #20149, #11319, #14734 ) ;
#7899 = ORIENTED_EDGE ( 'NONE', *, *, #3376, .T. ) ;
#7900 = DIRECTION ( 'NONE',  ( 0.000000000000000000, 0.000000000000000000, 1.000000000000000000 ) ) ;
#7901 = CARTESIAN_POINT ( 'NONE',  ( 5.004764015427562107, 40.00000000000000000, -51.61237785440702197 ) ) ;
#7902 = VECTOR ( 'NONE', #5532, 1000.000000000000000 ) ;
#7903 = VECTOR ( 'NONE', #4541, 1000.000000000000000 ) ;
#7904 = VERTEX_POINT ( 'NONE', #7364 ) ;
#7905 = CARTESIAN_POINT ( 'NONE',  ( 0.5471940025628014848, 39.99822778032481807, -49.15513688211015619 ) ) ;
#7906 = CONICAL_SURFACE ( 'NONE', #13731, 8.999999999999973355, 0.7853981633974657095 ) ;
#7907 = CARTESIAN_POINT ( 'NONE',  ( 2.602085213965210642E-15, 6.000000000000019540, 0.000000000000000000 ) ) ;
#7908 = EDGE_CURVE ( 'NONE', #8405, #8747, #9312, .T. ) ;
#7909 = B_SPLINE_CURVE_WITH_KNOTS ( 'NONE', 3,
 ( #18928, #3576, #5397, #3237 ),
 .UNSPECIFIED., .F., .F.,
 ( 4, 4 ),
 ( 0.001875451646902839224, 0.003761979286331241200 ),
 .UNSPECIFIED. ) ;
#7910 = DIRECTION ( 'NONE',  ( 0.8171172023792294681, -0.3308262969263033870, -0.4720947350246249008 ) ) ;
#7911 = CARTESIAN_POINT ( 'NONE',  ( -3.807409458091504995, 39.99999999999999289, 50.99570509775378468 ) ) ;
#7912 = CARTESIAN_POINT ( 'NONE',  ( -42.50000000000000711, -11.97499999999999964, -47.50000000000000000 ) ) ;
#7913 = CARTESIAN_POINT ( 'NONE',  ( 7.167333399831417102E-15, 39.99999999999997158, 48.73397172404483513 ) ) ;
#7914 = AXIS2_PLACEMENT_3D ( 'NONE', #16486, #793, #21765 ) ;
#7915 = CARTESIAN_POINT ( 'NONE',  ( 18.22261011550294185, 31.92986134326200443, 2.800654218530481465 ) ) ;
#7916 = ORIENTED_EDGE ( 'NONE', *, *, #5726, .T. ) ;
#7917 = DIRECTION ( 'NONE',  ( -0.000000000000000000, -1.000000000000000000, -0.000000000000000000 ) ) ;
#7918 = CARTESIAN_POINT ( 'NONE',  ( 4.936596639065565562, 31.11077005834400566, -6.999999999999950262 ) ) ;
#7919 = EDGE_CURVE ( 'NONE', #2308, #22537, #10627, .T. ) ;
#7920 = CARTESIAN_POINT ( 'NONE',  ( 35.00000000000000000, -9.000000000000001776, 4.258610482196280173E-15 ) ) ;
#7921 = ORIENTED_EDGE ( 'NONE', *, *, #2630, .F. ) ;
#7922 = CARTESIAN_POINT ( 'NONE',  ( -10.50000000000012079, 42.51666049839536043, 105.0000000000000142 ) ) ;
#7923 = CARTESIAN_POINT ( 'NONE',  ( 5.551115123125782702E-14, -1.387778780781445676E-13, -5.749999999999949374 ) ) ;
#7924 = AXIS2_PLACEMENT_3D ( 'NONE', #20209, #4514, #11495 ) ;
#7925 = VECTOR ( 'NONE', #13498, 1000.000000000000000 ) ;
#7926 = VERTEX_POINT ( 'NONE', #4159 ) ;
#7927 = CIRCLE ( 'NONE', #20737, 2.999999999999999112 ) ;
#7928 = ORIENTED_EDGE ( 'NONE', *, *, #18484, .F. ) ;
#7929 = ADVANCED_FACE ( 'NONE', ( #5638 ), #14101, .F. ) ;
#7930 = DIRECTION ( 'NONE',  ( 0.9999707308947706208, -0.006759637085566803406, 0.003583944788867206733 ) ) ;
#7931 = EDGE_LOOP ( 'NONE', ( #15803, #18692, #16940, #9255 ) ) ;
#7932 = CARTESIAN_POINT ( 'NONE',  ( 11.89435616776537508, 39.99999999999999289, 54.28884887643226165 ) ) ;
#7933 = CARTESIAN_POINT ( 'NONE',  ( 2.220446049250313081E-13, -8.326672684688674053E-14, 2.800654218530498785 ) ) ;
#7934 = FACE_OUTER_BOUND ( 'NONE', #3219, .T. ) ;
#7935 = DIRECTION ( 'NONE',  ( 0.000000000000000000, 0.000000000000000000, -1.000000000000000000 ) ) ;
#7936 = EDGE_CURVE ( 'NONE', #20516, #5386, #3339, .T. ) ;
#7937 = LINE ( 'NONE', #6439, #12727 ) ;
#7938 = ORIENTED_EDGE ( 'NONE', *, *, #476, .T. ) ;
#7939 = LINE ( 'NONE', #4280, #14594 ) ;
#7940 = CARTESIAN_POINT ( 'NONE',  ( -35.00000000000000000, 22.00000000000000355, 17.00000000000002487 ) ) ;
#7941 = ORIENTED_EDGE ( 'NONE', *, *, #11777, .T. ) ;
#7942 = CARTESIAN_POINT ( 'NONE',  ( 35.00000000000058265, 28.00000000000000000, -55.00000000000076028 ) ) ;
#7943 = VECTOR ( 'NONE', #354, 1000.000000000000000 ) ;
#7944 = DIRECTION ( 'NONE',  ( -0.000000000000000000, 1.000000000000000000, -0.000000000000000000 ) ) ;
#7945 = CARTESIAN_POINT ( 'NONE',  ( 35.00000000000000000, 40.00000000000000000, 4.258610482196280173E-15 ) ) ;
#7946 = VERTEX_POINT ( 'NONE', #14678 ) ;
#7947 = CARTESIAN_POINT ( 'NONE',  ( -4.406386027442511732, 39.99999999999999289, -51.31001915654736933 ) ) ;
#7948 = CARTESIAN_POINT ( 'NONE',  ( 1.255208329926582822, 39.96308463907303832, -50.19868133818717126 ) ) ;
#7949 = ORIENTED_EDGE ( 'NONE', *, *, #10273, .T. ) ;
#7950 = CARTESIAN_POINT ( 'NONE',  ( 2.576224933359583247, 39.84426458497860324, 51.65025110506229566 ) ) ;
#7951 = CARTESIAN_POINT ( 'NONE',  ( -2.589893228699289285, 0.1394114517735031977, -50.61995827140722781 ) ) ;
#7952 = AXIS2_PLACEMENT_3D ( 'NONE', #14340, #1881, #21130 ) ;
#7953 = EDGE_LOOP ( 'NONE', ( #1447, #12865, #17410, #2119 ) ) ;
#7954 = LINE ( 'NONE', #4176, #3948 ) ;
#7955 = CARTESIAN_POINT ( 'NONE',  ( 12.72045107882486370, 38.45933137995365314, 55.71167848415526436 ) ) ;
#7956 = CARTESIAN_POINT ( 'NONE',  ( -15.62726112422574332, -28.45046755804889216, 2.999999999999995559 ) ) ;
#7957 = EDGE_CURVE ( 'NONE', #22536, #4950, #18199, .T. ) ;
#7958 = EDGE_CURVE ( 'NONE', #9032, #3415, #9558, .T. ) ;
#7959 = CARTESIAN_POINT ( 'NONE',  ( 21.29213537401512468, 12.67546417994482688, -58.41859095437539651 ) ) ;
#7960 = VECTOR ( 'NONE', #116, 1000.000000000000000 ) ;
#7961 = CIRCLE ( 'NONE', #3199, 19.11328065563151668 ) ;
#7962 = VERTEX_POINT ( 'NONE', #4388 ) ;
#7963 = EDGE_LOOP ( 'NONE', ( #13873, #2006, #8237, #2537 ) ) ;
#7964 = EDGE_CURVE ( 'NONE', #6859, #7992, #16500, .T. ) ;
#7965 = EDGE_LOOP ( 'NONE', ( #485, #9414, #14427, #9420, #21581 ) ) ;
#7966 = ORIENTED_EDGE ( 'NONE', *, *, #5719, .F. ) ;
#7967 = DIRECTION ( 'NONE',  ( -0.000000000000000000, -0.000000000000000000, -1.000000000000000000 ) ) ;
#7968 = AXIS2_PLACEMENT_3D ( 'NONE', #4944, #13280, #8488 ) ;
#7969 = CIRCLE ( 'NONE', #6867, 2.500000000000002220 ) ;
#7970 = ORIENTED_EDGE ( 'NONE', *, *, #5719, .T. ) ;
#7971 = DIRECTION ( 'NONE',  ( 1.296372316667914327E-16, 1.000000000000000000, -0.000000000000000000 ) ) ;
#7972 = CARTESIAN_POINT ( 'NONE',  ( -34.99999999999999289, 0.000000000000000000, -5.000000000000030198 ) ) ;
#7973 = ORIENTED_EDGE ( 'NONE', *, *, #5785, .F. ) ;
#7974 = DIRECTION ( 'NONE',  ( 6.505213034913038160E-19, 3.903127820947822896E-18, 1.000000000000000000 ) ) ;
#7975 = ORIENTED_EDGE ( 'NONE', *, *, #18288, .T. ) ;
#7976 = CARTESIAN_POINT ( 'NONE',  ( -2.836563456948004695E-15, -1.236374842841498678, -48.24164917503444627 ) ) ;
#7977 = CARTESIAN_POINT ( 'NONE',  ( -34.99999999999999289, -5.000000000000000000, -57.49999999999705125 ) ) ;
#7978 = DIRECTION ( 'NONE',  ( 0.000000000000000000, 1.000000000000000000, 0.000000000000000000 ) ) ;
#7979 = AXIS2_PLACEMENT_3D ( 'NONE', #20500, #3082, #10051 ) ;
#7980 = CARTESIAN_POINT ( 'NONE',  ( -8.331955809010631597, 38.18181818181817988, -56.36098470834072316 ) ) ;
#7981 = ADVANCED_FACE ( 'NONE', ( #7934 ), #6100, .F. ) ;
#7982 = CARTESIAN_POINT ( 'NONE',  ( 25.00000000000000000, 20.00000000000000000, -16.49999999999997868 ) ) ;
#7983 = AXIS2_PLACEMENT_3D ( 'NONE', #9297, #18112, #2426 ) ;
#7984 = CARTESIAN_POINT ( 'NONE',  ( -32.14641817400179491, -18.83615802559812735, 3.000000000000023537 ) ) ;
#7985 = ORIENTED_EDGE ( 'NONE', *, *, #18946, .T. ) ;
#7986 = CIRCLE ( 'NONE', #8353, 19.99999999999999289 ) ;
#7987 = CIRCLE ( 'NONE', #12005, 0.9999999999999974465 ) ;
#7988 = VERTEX_POINT ( 'NONE', #12955 ) ;
#7989 = ADVANCED_FACE ( 'NONE', ( #16406 ), #16520, .F. ) ;
#7990 = CIRCLE ( 'NONE', #18236, 16.49999999999999645 ) ;
#7991 = CIRCLE ( 'NONE', #1033, 30.00000000000000000 ) ;
#7992 = VERTEX_POINT ( 'NONE', #15120 ) ;
#7993 = CARTESIAN_POINT ( 'NONE',  ( -19.03045156298755103, 26.21228714462430176, 57.88457068412354545 ) ) ;
#7994 = DIRECTION ( 'NONE',  ( -1.000000000000000000, -1.208970125616077665E-17, 0.000000000000000000 ) ) ;
#7995 = PLANE ( 'NONE',  #15643 ) ;
#7996 = CARTESIAN_POINT ( 'NONE',  ( -34.99999999999999289, -5.000000000000000000, -3.012171160963566127E-14 ) ) ;
#7997 = EDGE_CURVE ( 'NONE', #17762, #10374, #22371, .T. ) ;
#7998 = CARTESIAN_POINT ( 'NONE',  ( 31.11359284679396353, 4.918774254215635189, 2.999999999999995559 ) ) ;
#7999 = AXIS2_PLACEMENT_3D ( 'NONE', #6650, #6545, #845 ) ;
#8000 = FACE_OUTER_BOUND ( 'NONE', #21573, .T. ) ;
#8001 = CARTESIAN_POINT ( 'NONE',  ( 1.255529093608926727, 39.96306425836120724, 50.19904361858062458 ) ) ;
#8002 = CARTESIAN_POINT ( 'NONE',  ( 5.249999999999981348, 40.00000000000000000, 41.42387596543812123 ) ) ;
#8003 = CARTESIAN_POINT ( 'NONE',  ( 10.27431133777207961, -4.928932188134511172, 51.43682631505490832 ) ) ;
#8004 = DIRECTION ( 'NONE',  ( 0.000000000000000000, 0.000000000000000000, -1.000000000000000000 ) ) ;
#8005 = AXIS2_PLACEMENT_3D ( 'NONE', #3567, #17533, #14067 ) ;
#8006 = EDGE_CURVE ( 'NONE', #12299, #1894, #4734, .T. ) ;
#8007 = AXIS2_PLACEMENT_3D ( 'NONE', #2039, #19804, #21181 ) ;
#8008 = ORIENTED_EDGE ( 'NONE', *, *, #13426, .T. ) ;
#8009 = CARTESIAN_POINT ( 'NONE',  ( 35.00000000000000000, -9.000000000000001776, 4.258610482196280173E-15 ) ) ;
#8010 = CARTESIAN_POINT ( 'NONE',  ( -9.689843208404443686, 39.33333333333332860, 54.54983754392751649 ) ) ;
#8011 = DIRECTION ( 'NONE',  ( -6.505213034913038160E-19, -3.903127820947822896E-18, -1.000000000000000000 ) ) ;
#8012 = CARTESIAN_POINT ( 'NONE',  ( 35.00000000000000000, 25.00000000000000000, 2.365113165210053967E-14 ) ) ;
#8013 = AXIS2_PLACEMENT_3D ( 'NONE', #5178, #17416, #15355 ) ;
#8014 = EDGE_LOOP ( 'NONE', ( #21036, #18314, #12529, #9072 ) ) ;
#8015 = VERTEX_POINT ( 'NONE', #22139 ) ;
#8016 = DIRECTION ( 'NONE',  ( -6.505213034913038160E-19, -3.903127820947822896E-18, -1.000000000000000000 ) ) ;
#8017 = DIRECTION ( 'NONE',  ( 0.000000000000000000, 0.000000000000000000, -1.000000000000000000 ) ) ;
#8018 = AXIS2_PLACEMENT_3D ( 'NONE', #12566, #10972, #19577 ) ;
#8019 = DIRECTION ( 'NONE',  ( 0.000000000000000000, -0.7071067811867928210, -0.7071067811863022134 ) ) ;
#8020 = CARTESIAN_POINT ( 'NONE',  ( 8.421835294225278545, 39.99999999999998579, -53.12761979129442125 ) ) ;
#8021 = EDGE_CURVE ( 'NONE', #8747, #8574, #18246, .T. ) ;
#8022 = VERTEX_POINT ( 'NONE', #14787 ) ;
#8023 = CARTESIAN_POINT ( 'NONE',  ( 15.50000000000024336, -2.516660498395250301, -100.0000000000000000 ) ) ;
#8024 = DIRECTION ( 'NONE',  ( 0.000000000000000000, 1.000000000000000000, 0.000000000000000000 ) ) ;
#8025 = DIRECTION ( 'NONE',  ( 0.000000000000000000, -1.000000000000000000, 0.000000000000000000 ) ) ;
#8026 = CARTESIAN_POINT ( 'NONE',  ( -12.48541242016036357, 28.32175387455460935, -44.64471390988169475 ) ) ;
#8027 = EDGE_CURVE ( 'NONE', #15231, #11262, #9873, .T. ) ;
#8028 = AXIS2_PLACEMENT_3D ( 'NONE', #16705, #15075, #14965 ) ;
#8029 = VERTEX_POINT ( 'NONE', #13064 ) ;
#8030 = CARTESIAN_POINT ( 'NONE',  ( 33.52953626616073279, 9.708269511265299911, -2.999999999999999112 ) ) ;
#8031 = CARTESIAN_POINT ( 'NONE',  ( 35.00000000000001421, 5.000000000000000000, 1.540743955509788682E-30 ) ) ;
#8032 = FILL_AREA_STYLE_COLOUR ( '', #10946 ) ;
#8033 = CYLINDRICAL_SURFACE ( 'NONE', #5707, 2.499999999999996891 ) ;
#8034 = LINE ( 'NONE', #13266, #9995 ) ;
#8035 = ORIENTED_EDGE ( 'NONE', *, *, #20864, .F. ) ;
#8036 = CARTESIAN_POINT ( 'NONE',  ( 9.062586715441165452, 2.130694986412128511, 54.31128890270545639 ) ) ;
#8037 = FACE_OUTER_BOUND ( 'NONE', #4641, .T. ) ;
#8038 = DIRECTION ( 'NONE',  ( -6.505213034913038160E-19, -3.903127820947822896E-18, -1.000000000000000000 ) ) ;
#8039 = PRODUCT ( 'FLYWHEEL', 'FLYWHEEL', '', ( #19144 ) ) ;
#8040 = EDGE_CURVE ( 'NONE', #15365, #18812, #20083, .T. ) ;
#8041 = VERTEX_POINT ( 'NONE', #11703 ) ;
#8042 = MECHANICAL_DESIGN_GEOMETRIC_PRESENTATION_REPRESENTATION (  '', ( #2575 ), #11342 ) ;
#8043 = ORIENTED_EDGE ( 'NONE', *, *, #39, .T. ) ;
#8044 = DIRECTION ( 'NONE',  ( 0.9999707308947706208, -0.006759637085566771314, 0.003583944788867210636 ) ) ;
#8045 = ADVANCED_FACE ( 'NONE', ( #20309, #2443 ), #2897, .T. ) ;
#8046 = ORIENTED_EDGE ( 'NONE', *, *, #17374, .T. ) ;
#8047 = CARTESIAN_POINT ( 'NONE',  ( 18.52604901273056015, 27.59774142807036057, -60.25307787776290525 ) ) ;
#8048 = CARTESIAN_POINT ( 'NONE',  ( 90.00000000000000000, 28.00000000000000000, -9.108981535246192915E-16 ) ) ;
#8049 = CARTESIAN_POINT ( 'NONE',  ( 15.62726112422596714, 28.45046755804883531, -6.999999999999992006 ) ) ;
#8050 = CARTESIAN_POINT ( 'NONE',  ( -36.75746821813285692, 0.6841746959066752343, -2.800654218530457484 ) ) ;
#8051 = CARTESIAN_POINT ( 'NONE',  ( 5.833333333333437842, 6.180730040185884455, -40.61164310337073857 ) ) ;
#8052 = EDGE_LOOP ( 'NONE', ( #1676, #17404, #13963, #22249 ) ) ;
#8053 = CARTESIAN_POINT ( 'NONE',  ( -42.50000000000000711, -12.00000000000012434, 47.50000000000000711 ) ) ;
#8054 = CARTESIAN_POINT ( 'NONE',  ( 7.980461308159908285, -36.39375341857525825, -6.999999999999950262 ) ) ;
#8055 = ORIENTED_EDGE ( 'NONE', *, *, #16463, .F. ) ;
#8056 = DIRECTION ( 'NONE',  ( 0.000000000000000000, 0.5150380749100560429, 0.8571673007021112234 ) ) ;
#8057 = B_SPLINE_CURVE_WITH_KNOTS ( 'NONE', 3,
 ( #961, #19872, #2576, #21825 ),
 .UNSPECIFIED., .F., .F.,
 ( 4, 4 ),
 ( 9.715086409935858850E-07, 0.001929643240672463279 ),
 .UNSPECIFIED. ) ;
#8058 = CARTESIAN_POINT ( 'NONE',  ( 35.00000000000000000, 14.00000000000000000, -38.99999999999997868 ) ) ;
#8060 = VECTOR ( 'NONE', #16136, 1000.000000000000000 ) ;
#8059 = DIRECTION ( 'NONE',  ( 0.000000000000000000, 0.000000000000000000, -1.000000000000000000 ) ) ;
#8061 = CARTESIAN_POINT ( 'NONE',  ( 13.00000000000024336, -2.516660498395250745, 100.0000000000000000 ) ) ;
#8062 = ORIENTED_EDGE ( 'NONE', *, *, #10016, .T. ) ;
#8063 = CARTESIAN_POINT ( 'NONE',  ( -6.913287963588828688, 40.00000000000000711, -52.51234323549941507 ) ) ;
#8064 = DIRECTION ( 'NONE',  ( 0.000000000000000000, 0.000000000000000000, 1.000000000000000000 ) ) ;
#8065 = VERTEX_POINT ( 'NONE', #9644 ) ;
#8066 = CARTESIAN_POINT ( 'NONE',  ( 8.619966100995542391, 38.06590016575250246, 54.65505662632602224 ) ) ;
#8067 = CARTESIAN_POINT ( 'NONE',  ( -1.801805001521007421, 0.06845237652821531404, -51.82847917242283131 ) ) ;
#8068 = ORIENTED_EDGE ( 'NONE', *, *, #18691, .T. ) ;
#8069 = UNCERTAINTY_MEASURE_WITH_UNIT (LENGTH_MEASURE( 1.000000000000000082E-05 ), #3672, 'distance_accuracy_value', 'NONE');
#8070 = AXIS2_PLACEMENT_3D ( 'NONE', #75, #14028, #22680 ) ;
#8071 = CARTESIAN_POINT ( 'NONE',  ( -27.95348479018568355, 14.76298474240492276, -2.999999999999999112 ) ) ;
#8072 = FACE_OUTER_BOUND ( 'NONE', #10501, .T. ) ;
#8073 = EDGE_CURVE ( 'NONE', #6745, #6106, #6992, .T. ) ;
#8074 = CARTESIAN_POINT ( 'NONE',  ( 22.43750227530513186, 20.33721733310946433, -58.67013217117666102 ) ) ;
#8075 = EDGE_CURVE ( 'NONE', #20003, #16662, #20171, .T. ) ;
#8076 = ORIENTED_EDGE ( 'NONE', *, *, #13195, .F. ) ;
#8077 = CIRCLE ( 'NONE', #22358, 2.524999999999999467 ) ;
#8078 = ORIENTED_EDGE ( 'NONE', *, *, #4129, .F. ) ;
#8079 = VERTEX_POINT ( 'NONE', #4614 ) ;
#8080 = EDGE_CURVE ( 'NONE', #14890, #15747, #18588, .T. ) ;
#8081 = EDGE_CURVE ( 'NONE', #13677, #12296, #16127, .T. ) ;
#8082 = ORIENTED_EDGE ( 'NONE', *, *, #16095, .T. ) ;
#8083 = CARTESIAN_POINT ( 'NONE',  ( 10.84015308351855111, 39.16451817967297444, 54.95776488309492436 ) ) ;
#8084 = DIRECTION ( 'NONE',  ( -6.505213034913038160E-19, -3.903127820947822896E-18, -1.000000000000000000 ) ) ;
#8085 = ORIENTED_EDGE ( 'NONE', *, *, #7077, .T. ) ;
#8086 = CARTESIAN_POINT ( 'NONE',  ( 3.656418565264246467, 37.07861450834818129, -6.999999999999950262 ) ) ;
#8087 = CARTESIAN_POINT ( 'NONE',  ( -0.1993075991723092522, 13.00021308684595311, 6.999930029250709396 ) ) ;
#8088 = VERTEX_POINT ( 'NONE', #12150 ) ;
#8089 = CARTESIAN_POINT ( 'NONE',  ( -35.00000000000000000, -5.000000000000000000, 57.00000000000003553 ) ) ;
#8090 = EDGE_CURVE ( 'NONE', #3379, #12610, #7356, .T. ) ;
#8091 = CARTESIAN_POINT ( 'NONE',  ( 42.50000000000000711, -3.738192700042122674, -47.50000000000000000 ) ) ;
#8092 = ORIENTED_EDGE ( 'NONE', *, *, #9036, .F. ) ;
#8093 = CARTESIAN_POINT ( 'NONE',  ( -9.103081159019573931, 0.03030367950605317509, -53.87333532811887693 ) ) ;
#8094 = ADVANCED_FACE ( 'NONE', ( #22482 ), #3347, .T. ) ;
#8095 = FACE_OUTER_BOUND ( 'NONE', #1974, .T. ) ;
#8096 = LINE ( 'NONE', #18389, #1313 ) ;
#8097 = DIRECTION ( 'NONE',  ( 8.659560562354903276E-17, -0.7071067811865500152, 0.7071067811865451302 ) ) ;
#8098 = CIRCLE ( 'NONE', #4802, 1.000000000000000888 ) ;
#8099 = CARTESIAN_POINT ( 'NONE',  ( 90.00000000000000000, 40.00000000000000711, 2.524999999999998579 ) ) ;
#8100 = EDGE_LOOP ( 'NONE', ( #14475, #1564, #7446, #10597, #15862 ) ) ;
#8101 = EDGE_LOOP ( 'NONE', ( #965, #15077, #19109, #13023 ) ) ;
#8102 = ORIENTED_EDGE ( 'NONE', *, *, #12330, .F. ) ;
#8103 = CARTESIAN_POINT ( 'NONE',  ( -15.99370094303835899, 7.960486082690917620, 59.50964696497263873 ) ) ;
#8104 = DIRECTION ( 'NONE',  ( 6.505213034913038160E-19, 3.903127820947822896E-18, 1.000000000000000000 ) ) ;
#8105 = FACE_OUTER_BOUND ( 'NONE', #10982, .T. ) ;
#8106 = DIRECTION ( 'NONE',  ( 0.000000000000000000, 0.000000000000000000, 1.000000000000000000 ) ) ;
#8107 = ADVANCED_FACE ( 'NONE', ( #1733 ), #20977, .F. ) ;
#8108 = EDGE_CURVE ( 'NONE', #11717, #11286, #17076, .T. ) ;
#8109 = FACE_OUTER_BOUND ( 'NONE', #267, .T. ) ;
#8110 = ORIENTED_EDGE ( 'NONE', *, *, #10469, .T. ) ;
#8111 = DIRECTION ( 'NONE',  ( 6.505213034913038160E-19, 3.903127820947822896E-18, 1.000000000000000000 ) ) ;
#8112 = CARTESIAN_POINT ( 'NONE',  ( 5.302825731643186380, 39.28770244913255993, 54.25167596405761117 ) ) ;
#8113 = CARTESIAN_POINT ( 'NONE',  ( -13.56354382738803999, 2.142135623730931471, -56.03997097393684612 ) ) ;
#8114 = CARTESIAN_POINT ( 'NONE',  ( -4.278324951949648458, 39.54020021135842455, -53.33400390259981805 ) ) ;
#8115 = CIRCLE ( 'NONE', #17979, 2.500000000000002220 ) ;
#8116 = ORIENTED_EDGE ( 'NONE', *, *, #18280, .F. ) ;
#8117 = ADVANCED_FACE ( 'NONE', ( #3111 ), #4834, .F. ) ;
#8118 = DIRECTION ( 'NONE',  ( 0.000000000000000000, 0.000000000000000000, 1.000000000000000000 ) ) ;
#8119 = DIRECTION ( 'NONE',  ( 1.000000000000000000, 0.000000000000000000, 0.000000000000000000 ) ) ;
#8120 = CARTESIAN_POINT ( 'NONE',  ( -15.50000000000011013, 42.51666049839536043, -105.0000000000000142 ) ) ;
#8121 = ORIENTED_EDGE ( 'NONE', *, *, #7501, .T. ) ;
#8122 = DIRECTION ( 'NONE',  ( 0.000000000000000000, 0.000000000000000000, -1.000000000000000000 ) ) ;
#8123 = DIRECTION ( 'NONE',  ( 6.505213034913038160E-19, 3.903127820947822896E-18, 1.000000000000000000 ) ) ;
#8124 = DIRECTION ( 'NONE',  ( 0.000000000000000000, -1.000000000000000000, 0.000000000000000000 ) ) ;
#8125 = ORIENTED_EDGE ( 'NONE', *, *, #2596, .F. ) ;
#8126 = ORIENTED_EDGE ( 'NONE', *, *, #18779, .T. ) ;
#8127 = CARTESIAN_POINT ( 'NONE',  ( -7.486329337576093756, -0.2507164912831579828, 53.02637754495041378 ) ) ;
#8128 = EDGE_CURVE ( 'NONE', #8181, #5732, #10602, .T. ) ;
#8129 = AXIS2_PLACEMENT_3D ( 'NONE', #2420, #7684, #12933 ) ;
#8130 = DIRECTION ( 'NONE',  ( 0.000000000000000000, 0.000000000000000000, -1.000000000000000000 ) ) ;
#8131 = ORIENTED_EDGE ( 'NONE', *, *, #8513, .T. ) ;
#8132 = CARTESIAN_POINT ( 'NONE',  ( 21.65063509461090518, 12.49999999999978861, 2.999999999999995559 ) ) ;
#8133 = DIRECTION ( 'NONE',  ( 0.000000000000000000, 0.000000000000000000, 1.000000000000000000 ) ) ;
#8134 = CARTESIAN_POINT ( 'NONE',  ( -4.846083821622991117, 40.00000000000000711, 51.53252581920469311 ) ) ;
#8135 = CARTESIAN_POINT ( 'NONE',  ( 11.86180952234342278, 38.99999999999291589, -55.35904751185374550 ) ) ;
#8136 = CARTESIAN_POINT ( 'NONE',  ( 42.50000000000000711, -12.00000000000000000, 41.00000000000000711 ) ) ;
#8137 = LINE ( 'NONE', #15097, #9216 ) ;
#8138 = ORIENTED_EDGE ( 'NONE', *, *, #11870, .T. ) ;
#8139 = DIRECTION ( 'NONE',  ( 0.000000000000000000, -1.000000000000000000, 0.000000000000000000 ) ) ;
#8140 = DIRECTION ( 'NONE',  ( 0.000000000000000000, 0.000000000000000000, 1.000000000000000000 ) ) ;
#8141 = CARTESIAN_POINT ( 'NONE',  ( 9.744263423234823307, 2.495070046653235174, -54.63687069582775280 ) ) ;
#8142 = CYLINDRICAL_SURFACE ( 'NONE', #21362, 1.000000000000000888 ) ;
#8143 = ORIENTED_EDGE ( 'NONE', *, *, #11989, .F. ) ;
#8144 = AXIS2_PLACEMENT_3D ( 'NONE', #13800, #20819, #11864 ) ;
#8145 = DIRECTION ( 'NONE',  ( 0.000000000000000000, 1.000000000000000000, 0.000000000000000000 ) ) ;
#8146 = DIRECTION ( 'NONE',  ( 0.000000000000000000, 0.000000000000000000, -1.000000000000000000 ) ) ;
#8147 = EDGE_CURVE ( 'NONE', #14794, #21010, #10966, .T. ) ;
#8148 = ORIENTED_EDGE ( 'NONE', *, *, #12598, .F. ) ;
#8149 = EDGE_CURVE ( 'NONE', #12680, #2120, #17564, .T. ) ;
#8150 = ORIENTED_EDGE ( 'NONE', *, *, #15486, .F. ) ;
#8151 = DIRECTION ( 'NONE',  ( 0.000000000000000000, 0.000000000000000000, 1.000000000000000000 ) ) ;
#8152 = EDGE_LOOP ( 'NONE', ( #14009, #2806, #19500, #1309, #16780 ) ) ;
#8153 = CARTESIAN_POINT ( 'NONE',  ( 10.15869103000891549, 39.99999999999999289, 53.70409622859173027 ) ) ;
#8154 = DIRECTION ( 'NONE',  ( 0.9012767464701768594, -2.395770963567785064E-16, -0.4332438415859278247 ) ) ;
#8155 = CARTESIAN_POINT ( 'NONE',  ( -1.387778780781445676E-14, 20.00000000000000000, 101.0000000000000568 ) ) ;
#8156 = CARTESIAN_POINT ( 'NONE',  ( 19.80807096600698358, 16.80592363802972145, 60.57763526510201757 ) ) ;
#8157 = DIRECTION ( 'NONE',  ( -6.505213034913038160E-19, -3.903127820947822896E-18, -1.000000000000000000 ) ) ;
#8158 = ORIENTED_EDGE ( 'NONE', *, *, #7323, .T. ) ;
#8159 = DIRECTION ( 'NONE',  ( 0.000000000000000000, 0.000000000000000000, -1.000000000000000000 ) ) ;
#8160 = CARTESIAN_POINT ( 'NONE',  ( -35.00000000000000000, 17.00000000000000000, -40.99999999999997868 ) ) ;
#8161 = ORIENTED_EDGE ( 'NONE', *, *, #17834, .F. ) ;
#8162 = CARTESIAN_POINT ( 'NONE',  ( -13.08927703801866649, 12.63446361230555581, -44.94509734929665967 ) ) ;
#8163 = AXIS2_PLACEMENT_3D ( 'NONE', #962, #16542, #13421 ) ;
#8164 = CARTESIAN_POINT ( 'NONE',  ( 35.00000000000001421, 0.000000000000000000, 11.00000000000003730 ) ) ;
#8165 = DIRECTION ( 'NONE',  ( 0.000000000000000000, -1.000000000000000000, 0.000000000000000000 ) ) ;
#8166 = LINE ( 'NONE', #22151, #19604 ) ;
#8167 = ORIENTED_EDGE ( 'NONE', *, *, #21962, .T. ) ;
#8168 = LINE ( 'NONE', #2912, #18086 ) ;
#8169 = ADVANCED_FACE ( 'NONE', ( #18809 ), #3004, .F. ) ;
#8170 = ORIENTED_EDGE ( 'NONE', *, *, #14597, .T. ) ;
#8171 = CARTESIAN_POINT ( 'NONE',  ( -42.50000000000000000, 10.00000000000000000, 47.49999999999999289 ) ) ;
#8172 = CARTESIAN_POINT ( 'NONE',  ( 0.05289805390978788435, -1.234055917683787085, -48.20418456595464107 ) ) ;
#8173 = ORIENTED_EDGE ( 'NONE', *, *, #11678, .T. ) ;
#8174 = DIRECTION ( 'NONE',  ( -0.000000000000000000, -1.000000000000000000, -0.000000000000000000 ) ) ;
#8175 = DIRECTION ( 'NONE',  ( 0.000000000000000000, 1.000000000000000000, 0.000000000000000000 ) ) ;
#8176 = DIRECTION ( 'NONE',  ( 6.505213034913038160E-19, 3.903127820947822896E-18, 1.000000000000000000 ) ) ;
#8177 = EDGE_CURVE ( 'NONE', #13151, #14094, #14976, .T. ) ;
#8178 = AXIS2_PLACEMENT_3D ( 'NONE', #14362, #18163, #3849 ) ;
#8179 = CARTESIAN_POINT ( 'NONE',  ( 19.98510692294565771, 21.15566478732735689, -58.14357129517338052 ) ) ;
#8180 = CIRCLE ( 'NONE', #1218, 49.99999999999998579 ) ;
#8181 = VERTEX_POINT ( 'NONE', #8598 ) ;
#8182 = VERTEX_POINT ( 'NONE', #8381 ) ;
#8183 = VERTEX_POINT ( 'NONE', #19040 ) ;
#8184 = ORIENTED_EDGE ( 'NONE', *, *, #1905, .T. ) ;
#8185 = CARTESIAN_POINT ( 'NONE',  ( 0.9710767271268372358, 24.84180973946540405, 6.949333411110966807 ) ) ;
#8186 = VECTOR ( 'NONE', #18167, 1000.000000000000000 ) ;
#8187 = EDGE_LOOP ( 'NONE', ( #563, #4634, #11413, #16126 ) ) ;
#8188 = DIRECTION ( 'NONE',  ( -1.000000000000000000, 1.371829164384562918E-16, 0.000000000000000000 ) ) ;
#8189 = CARTESIAN_POINT ( 'NONE',  ( -2.394928258197305482, 14.15236082731613010, 6.680059847329907541 ) ) ;
#8190 = VERTEX_POINT ( 'NONE', #15352 ) ;
#8191 = CARTESIAN_POINT ( 'NONE',  ( 42.50000000000000000, 7.000000000000000000, 47.49999999999999289 ) ) ;
#8192 = CARTESIAN_POINT ( 'NONE',  ( 13.85640646055130709, -1.500000000000015099, -8.000000000000097700 ) ) ;
#8193 = CIRCLE ( 'NONE', #21003, 19.11328065563151668 ) ;
#8194 = EDGE_CURVE ( 'NONE', #20949, #2722, #5865, .T. ) ;
#8195 = EDGE_LOOP ( 'NONE', ( #8505, #12511 ) ) ;
#8196 = CARTESIAN_POINT ( 'NONE',  ( 9.375626977035830478, 39.53999066946833096, -54.37753981121610281 ) ) ;
#8197 = CIRCLE ( 'NONE', #10736, 2.099999999999990763 ) ;
#8198 = FACE_OUTER_BOUND ( 'NONE', #3486, .T. ) ;
#8199 = CARTESIAN_POINT ( 'NONE',  ( -9.038247590030331514E-14, -2.816400600653316655, -47.26426760038560104 ) ) ;
#8200 = CARTESIAN_POINT ( 'NONE',  ( -0.04595184375223184542, 40.00000000000000711, 48.76974637106872024 ) ) ;
#8201 = AXIS2_PLACEMENT_3D ( 'NONE', #17406, #22360, #1604 ) ;
#8202 = EDGE_CURVE ( 'NONE', #13043, #8088, #19032, .T. ) ;
#8203 = ADVANCED_FACE ( 'NONE', ( #22372 ), #2195, .F. ) ;
#8204 = AXIS2_PLACEMENT_3D ( 'NONE', #5446, #10687, #19431 ) ;
#8205 = CARTESIAN_POINT ( 'NONE',  ( -13.75658951623323745, 14.00814961052206797, 45.26303799332217892 ) ) ;
#8206 = ORIENTED_EDGE ( 'NONE', *, *, #19432, .F. ) ;
#8207 = CIRCLE ( 'NONE', #21021, 6.499999999999999112 ) ;
#8208 = ORIENTED_EDGE ( 'NONE', *, *, #4776, .T. ) ;
#8209 = EDGE_CURVE ( 'NONE', #17260, #651, #7310, .T. ) ;
#8210 = MECHANICAL_DESIGN_GEOMETRIC_PRESENTATION_REPRESENTATION (  '', ( #15508 ), #15874 ) ;
#8211 = ORIENTED_EDGE ( 'NONE', *, *, #13900, .F. ) ;
#8212 = CARTESIAN_POINT ( 'NONE',  ( -18.85220035179115072, 32.22744690108881116, 57.78902400853742449 ) ) ;
#8213 = CARTESIAN_POINT ( 'NONE',  ( -90.00000000000000000, 26.00000000000000355, -9.108981535246192915E-16 ) ) ;
#8214 = CARTESIAN_POINT ( 'NONE',  ( -13.85640646055084702, -25.00000000000000000, 11.99999999999970335 ) ) ;
#8215 = CARTESIAN_POINT ( 'NONE',  ( -11.77933723464119531, 39.99999999999998579, 54.24924979334856090 ) ) ;
#8216 = EDGE_LOOP ( 'NONE', ( #19479, #4957, #15945, #5387 ) ) ;
#8217 = AXIS2_PLACEMENT_3D ( 'NONE', #13075, #11819, #15022 ) ;
#8218 = CYLINDRICAL_SURFACE ( 'NONE', #2521, 36.76383501243555685 ) ;
#8219 = CARTESIAN_POINT ( 'NONE',  ( -3.397749879293104236, 40.00000000000000711, -50.77335388622131518 ) ) ;
#8220 = CARTESIAN_POINT ( 'NONE',  ( -0.2854126906104058614, -4.332981472378775401, 48.52899265465749323 ) ) ;
#8221 = DIRECTION ( 'NONE',  ( 0.000000000000000000, 0.000000000000000000, 1.000000000000000000 ) ) ;
#8222 = AXIS2_PLACEMENT_3D ( 'NONE', #9939, #13699, #17038 ) ;
#8223 = ORIENTED_EDGE ( 'NONE', *, *, #11640, .F. ) ;
#8224 = CARTESIAN_POINT ( 'NONE',  ( -10.71765026552324152, 39.18334136345070107, 54.91251049719502220 ) ) ;
#8225 = CARTESIAN_POINT ( 'NONE',  ( -27.95348479018550591, 14.76298474240492276, -6.999999999999950262 ) ) ;
#8226 = EDGE_LOOP ( 'NONE', ( #7685, #13794, #19507, #11734 ) ) ;
#8227 = CARTESIAN_POINT ( 'NONE',  ( 90.00000000000000000, 40.00000000000000711, -2.525000000000000355 ) ) ;
#8228 = DIRECTION ( 'NONE',  ( 0.000000000000000000, 0.000000000000000000, -1.000000000000000000 ) ) ;
#8229 = LINE ( 'NONE', #8342, #11573 ) ;
#8230 = ADVANCED_FACE ( 'NONE', ( #10417 ), #10, .F. ) ;
#8231 = VERTEX_POINT ( 'NONE', #21093 ) ;
#8232 = EDGE_CURVE ( 'NONE', #12856, #353, #5140, .T. ) ;
#8233 = EDGE_LOOP ( 'NONE', ( #17203, #16857, #11709, #19544 ) ) ;
#8234 = FACE_OUTER_BOUND ( 'NONE', #326, .T. ) ;
#8235 = ADVANCED_FACE ( 'NONE', ( #21425, #2287 ), #7103, .T. ) ;
#8236 = DIRECTION ( 'NONE',  ( -6.505213034913038160E-19, -3.903127820947822896E-18, -1.000000000000000000 ) ) ;
#8237 = ORIENTED_EDGE ( 'NONE', *, *, #15184, .T. ) ;
#8238 = CARTESIAN_POINT ( 'NONE',  ( 17.66631876130941947, -31.41173278719250206, -6.999999999999950262 ) ) ;
#8239 = CARTESIAN_POINT ( 'NONE',  ( -2.601474714586578418, 34.77495088821684277, -39.07471001004991962 ) ) ;
#8240 = DIRECTION ( 'NONE',  ( -6.505213034913038160E-19, -3.903127820947822896E-18, -1.000000000000000000 ) ) ;
#8241 = CIRCLE ( 'NONE', #13701, 31.50000000000001421 ) ;
#8242 = CARTESIAN_POINT ( 'NONE',  ( -17.42297160866542427, 10.14068842408707560, -59.94615209474301309 ) ) ;
#8243 = CARTESIAN_POINT ( 'NONE',  ( -1.486423889133612786, 39.99051292429980009, 49.86506860348632841 ) ) ;
#8244 = VECTOR ( 'NONE', #3771, 1000.000000000000114 ) ;
#8245 = DIRECTION ( 'NONE',  ( -0.000000000000000000, 1.000000000000000000, -0.000000000000000000 ) ) ;
#8246 = ORIENTED_EDGE ( 'NONE', *, *, #12898, .T. ) ;
#8247 = DIRECTION ( 'NONE',  ( -1.000000000000000000, 0.000000000000000000, 0.000000000000000000 ) ) ;
#8248 = DIRECTION ( 'NONE',  ( 0.000000000000000000, 0.000000000000000000, 1.000000000000000000 ) ) ;
#8249 = CARTESIAN_POINT ( 'NONE',  ( -34.65667543218827973, -4.170748987303380062, 3.000000000000002665 ) ) ;
#8250 = VECTOR ( 'NONE', #19557, 1000.000000000000000 ) ;
#8251 = EDGE_LOOP ( 'NONE', ( #15323, #3397, #17017, #17439 ) ) ;
#8252 = LINE ( 'NONE', #20517, #4698 ) ;
#8253 = CARTESIAN_POINT ( 'NONE',  ( -7.196011215416630691, -35.43002037646316182, -2.933296326616338767 ) ) ;
#8254 = CARTESIAN_POINT ( 'NONE',  ( -28.95348479018568355, 14.76298474240497782, -2.999999999999999112 ) ) ;
#8255 = CYLINDRICAL_SURFACE ( 'NONE', #14926, 60.00000000000000000 ) ;
#8256 = VECTOR ( 'NONE', #15816, 1000.000000000000114 ) ;
#8257 = ORIENTED_EDGE ( 'NONE', *, *, #19893, .F. ) ;
#8258 = VECTOR ( 'NONE', #10124, 1000.000000000000000 ) ;
#8259 = CIRCLE ( 'NONE', #5693, 2.500000000000002220 ) ;
#8260 = ORIENTED_EDGE ( 'NONE', *, *, #6689, .T. ) ;
#8261 = CIRCLE ( 'NONE', #2416, 36.76383501243555685 ) ;
#8262 = ORIENTED_EDGE ( 'NONE', *, *, #17392, .F. ) ;
#8263 = DIRECTION ( 'NONE',  ( 6.505213034913038160E-19, 3.903127820947822896E-18, 1.000000000000000000 ) ) ;
#8264 = VECTOR ( 'NONE', #21537, 1000.000000000000000 ) ;
#8265 = CARTESIAN_POINT ( 'NONE',  ( 8.306841138038604910, 0.005341471399264901936, 53.48947974206469524 ) ) ;
#8266 = CARTESIAN_POINT ( 'NONE',  ( 2.775557561562891351E-14, -2.775557561562891351E-14, 2.999999999999999112 ) ) ;
#8267 = FACE_OUTER_BOUND ( 'NONE', #6768, .T. ) ;
#8268 = CARTESIAN_POINT ( 'NONE',  ( -1.387778780781445518E-14, 20.00000000000000355, 105.0000000000000142 ) ) ;
#8269 = ORIENTED_EDGE ( 'NONE', *, *, #11404, .T. ) ;
#8270 = DIRECTION ( 'NONE',  ( -1.000000000000000000, 6.171687555462485044E-15, 0.000000000000000000 ) ) ;
#8271 = CARTESIAN_POINT ( 'NONE',  ( -1.387778780781445676E-14, 20.00000000000000000, 100.0000000000000000 ) ) ;
#8272 = ORIENTED_EDGE ( 'NONE', *, *, #8801, .T. ) ;
#8273 = CARTESIAN_POINT ( 'NONE',  ( -15.00000000000001421, 20.00000000000000000, -45.82575694955838230 ) ) ;
#8274 = ADVANCED_FACE ( 'NONE', ( #3685 ), #571, .T. ) ;
#8275 = DIRECTION ( 'NONE',  ( 0.000000000000000000, -0.000000000000000000, -1.000000000000000000 ) ) ;
#8276 = LINE ( 'NONE', #18597, #13344 ) ;
#8277 = CARTESIAN_POINT ( 'NONE',  ( 2.633052075911578527, 39.95897179782880926, 50.67294416386110356 ) ) ;
#8278 = ORIENTED_EDGE ( 'NONE', *, *, #5324, .F. ) ;
#8279 = CARTESIAN_POINT ( 'NONE',  ( -6.490531301833351918, 40.00000000000000711, -52.32367560554533270 ) ) ;
#8280 = ORIENTED_EDGE ( 'NONE', *, *, #19742, .F. ) ;
#8281 = FACE_OUTER_BOUND ( 'NONE', #10213, .T. ) ;
#8282 = VECTOR ( 'NONE', #17454, 1000.000000000000000 ) ;
#8283 = CIRCLE ( 'NONE', #3901, 6.499999999999999112 ) ;
#8284 = CARTESIAN_POINT ( 'NONE',  ( -2.836563456948004695E-15, -1.236374842841498678, -48.24164917503444627 ) ) ;
#8285 = VECTOR ( 'NONE', #10647, 1000.000000000000000 ) ;
#8286 = EDGE_LOOP ( 'NONE', ( #6013, #22051, #6057, #15770 ) ) ;
#8287 = CARTESIAN_POINT ( 'NONE',  ( 35.00000000000000000, 40.00000000000000000, 4.258610482196280173E-15 ) ) ;
#8288 = ADVANCED_FACE ( 'NONE', ( #7443 ), #21549, .F. ) ;
#8289 = LINE ( 'NONE', #22390, #199 ) ;
#8290 = CARTESIAN_POINT ( 'NONE',  ( -35.00000000000000000, 17.00000000000000000, -40.99999999999997868 ) ) ;
#8291 = VECTOR ( 'NONE', #9392, 1000.000000000000000 ) ;
#8292 = CARTESIAN_POINT ( 'NONE',  ( 19.03045156299229745, 26.21228714462666787, -57.88457068413015350 ) ) ;
#8293 = ORIENTED_EDGE ( 'NONE', *, *, #22450, .T. ) ;
#8294 = ORIENTED_EDGE ( 'NONE', *, *, #14501, .F. ) ;
#8295 = ORIENTED_EDGE ( 'NONE', *, *, #17139, .T. ) ;
#8296 = CARTESIAN_POINT ( 'NONE',  ( 12.00000000000000355, 1.500000000000003553, 0.000000000000000000 ) ) ;
#8297 = AXIS2_PLACEMENT_3D ( 'NONE', #8813, #1717, #10289 ) ;
#8298 = ORIENTED_EDGE ( 'NONE', *, *, #12132, .F. ) ;
#8299 = DIRECTION ( 'NONE',  ( 1.000000000000000000, 0.000000000000000000, 0.000000000000000000 ) ) ;
#8300 = ORIENTED_EDGE ( 'NONE', *, *, #12855, .T. ) ;
#8301 = CARTESIAN_POINT ( 'NONE',  ( -42.49999999999996447, 10.00000000000000000, -47.50000000000000711 ) ) ;
#8302 = CARTESIAN_POINT ( 'NONE',  ( -2.999929132934958886, 15.60292843345686187, 6.485306429529695826 ) ) ;
#8303 = ORIENTED_EDGE ( 'NONE', *, *, #18398, .T. ) ;
#8304 = EDGE_CURVE ( 'NONE', #8525, #16794, #17928, .T. ) ;
#8305 = CARTESIAN_POINT ( 'NONE',  ( -22.28024240313483517, -22.26748298433275863, -6.999999999999957367 ) ) ;
#8306 = CIRCLE ( 'NONE', #5374, 6.499999999999999112 ) ;
#8307 = VERTEX_POINT ( 'NONE', #12583 ) ;
#8308 = CARTESIAN_POINT ( 'NONE',  ( 4.750176626998272589, 39.43750955791287538, -52.76318975003094636 ) ) ;
#8309 = LINE ( 'NONE', #14551, #13102 ) ;
#8310 = FACE_OUTER_BOUND ( 'NONE', #7847, .T. ) ;
#8311 = CARTESIAN_POINT ( 'NONE',  ( 1.387778780781445676E-14, 40.00000000000000000, 48.73397172404482802 ) ) ;
#8312 = ADVANCED_FACE ( 'NONE', ( #12260 ), #5390, .F. ) ;
#8313 = VECTOR ( 'NONE', #15360, 1000.000000000000000 ) ;
#8314 = CIRCLE ( 'NONE', #10864, 19.11328065563151668 ) ;
#8315 = DIRECTION ( 'NONE',  ( -0.7071067811865522357, 8.080682403282904861E-17, 0.7071067811865429098 ) ) ;
#8316 = EDGE_LOOP ( 'NONE', ( #3813, #17396 ) ) ;
#8317 = ORIENTED_EDGE ( 'NONE', *, *, #6047, .F. ) ;
#8318 = ADVANCED_FACE ( 'NONE', ( #4029 ), #10532, .F. ) ;
#8319 = ORIENTED_EDGE ( 'NONE', *, *, #7605, .F. ) ;
#8320 = ORIENTED_EDGE ( 'NONE', *, *, #18843, .F. ) ;
#8321 = CARTESIAN_POINT ( 'NONE',  ( -19.96824854984944508, 18.58379861519951959, 58.13906733437337948 ) ) ;
#8322 = CARTESIAN_POINT ( 'NONE',  ( 3.330669073875469621E-13, -1.110223024625156540E-13, -2.999999999999971578 ) ) ;
#8323 = VECTOR ( 'NONE', #19272, 1000.000000000000000 ) ;
#8324 = AXIS2_PLACEMENT_3D ( 'NONE', #20033, #4339, #11318 ) ;
#8325 = CARTESIAN_POINT ( 'NONE',  ( 35.00000000000001421, 1.000000000000044187, 1.540743955509788682E-30 ) ) ;
#8326 = CARTESIAN_POINT ( 'NONE',  ( 8.230913578179089640, 39.55470086212452685, 53.98103023414088142 ) ) ;
#8327 = EDGE_CURVE ( 'NONE', #11150, #12296, #8934, .T. ) ;
#8328 = CIRCLE ( 'NONE', #1018, 15.99999999999993072 ) ;
#8329 = DIRECTION ( 'NONE',  ( -1.000000000000000000, -1.208970125616044077E-17, 0.000000000000000000 ) ) ;
#8330 = ORIENTED_EDGE ( 'NONE', *, *, #7859, .T. ) ;
#8331 = DIRECTION ( 'NONE',  ( -0.000000000000000000, 1.000000000000000000, -0.000000000000000000 ) ) ;
#8332 = CARTESIAN_POINT ( 'NONE',  ( -4.643077448496365278, 40.00000000000000711, -51.42938343542150648 ) ) ;
#8333 = CARTESIAN_POINT ( 'NONE',  ( 3.330669073875469621E-13, -1.110223024625156540E-13, -2.999999999999971578 ) ) ;
#8334 = EDGE_LOOP ( 'NONE', ( #17450, #2574, #3016, #1919 ) ) ;
#8335 = AXIS2_PLACEMENT_3D ( 'NONE', #13874, #8616, #20892 ) ;
#8336 = EDGE_CURVE ( 'NONE', #938, #5289, #5494, .T. ) ;
#8337 = DIRECTION ( 'NONE',  ( 0.000000000000000000, 0.000000000000000000, -1.000000000000000000 ) ) ;
#8338 = EDGE_LOOP ( 'NONE', ( #2449, #8407, #20845, #3103 ) ) ;
#8339 = CIRCLE ( 'NONE', #19701, 6.499999999999999112 ) ;
#8340 = CARTESIAN_POINT ( 'NONE',  ( -10.27431133777641215, -4.928932188134511172, -51.43682631505697600 ) ) ;
#8341 = AXIS2_PLACEMENT_3D ( 'NONE', #8333, #13575, #12108 ) ;
#8342 = CARTESIAN_POINT ( 'NONE',  ( 31.41239365194212141, -2.347663744114298012, -6.999999999999999112 ) ) ;
#8343 = ADVANCED_FACE ( 'NONE', ( #1845 ), #108, .F. ) ;
#8344 = AXIS2_PLACEMENT_3D ( 'NONE', #20252, #6720, #11536 ) ;
#8345 = ORIENTED_EDGE ( 'NONE', *, *, #5866, .T. ) ;
#8346 = EDGE_CURVE ( 'NONE', #4117, #16727, #1816, .T. ) ;
#8347 = EDGE_LOOP ( 'NONE', ( #14357, #1396 ) ) ;
#8348 = CARTESIAN_POINT ( 'NONE',  ( -5.974741775054217996, -3.061019228945407455, 51.30674412914550686 ) ) ;
#8349 = AXIS2_PLACEMENT_3D ( 'NONE', #12801, #2395, #13359 ) ;
#8350 = CARTESIAN_POINT ( 'NONE',  ( -42.50000000000000711, -12.00000000000012434, -47.50000000000000000 ) ) ;
#8351 = EDGE_CURVE ( 'NONE', #16045, #3371, #15343, .T. ) ;
#8352 = ORIENTED_EDGE ( 'NONE', *, *, #4590, .F. ) ;
#8353 = AXIS2_PLACEMENT_3D ( 'NONE', #17451, #15386, #5106 ) ;
#8354 = CIRCLE ( 'NONE', #1412, 41.25806096964028313 ) ;
#8355 = CYLINDRICAL_SURFACE ( 'NONE', #13540, 19.11328065563151668 ) ;
#8356 = CONICAL_SURFACE ( 'NONE', #4346, 58.99999999999994316, 0.7853981633974725929 ) ;
#8357 = CARTESIAN_POINT ( 'NONE',  ( 35.00000000000000000, 14.00000000000000000, -38.99999999999997868 ) ) ;
#8358 = CARTESIAN_POINT ( 'NONE',  ( 10.01544929272322548, -34.09574698892478750, 3.000000000000064837 ) ) ;
#8359 = CARTESIAN_POINT ( 'NONE',  ( -17.58064943503768518, 10.42262370234541358, -57.45835854660190023 ) ) ;
#8360 = AXIS2_PLACEMENT_3D ( 'NONE', #22259, #11925, #13518 ) ;
#8361 = EDGE_CURVE ( 'NONE', #1555, #15098, #12076, .T. ) ;
#8362 = CARTESIAN_POINT ( 'NONE',  ( 25.99999999999998579, 19.99999999999999645, 100.0000000000000000 ) ) ;
#8363 = CARTESIAN_POINT ( 'NONE',  ( -9.165377225651191395, 37.79989650906291132, 54.16098472236624417 ) ) ;
#8364 = VERTEX_POINT ( 'NONE', #14301 ) ;
#8365 = FACE_OUTER_BOUND ( 'NONE', #15202, .T. ) ;
#8366 = FACE_BOUND ( 'NONE', #13680, .T. ) ;
#8367 = CARTESIAN_POINT ( 'NONE',  ( 11.68090480754619875, 3.765577839755218648, -57.90797000640169045 ) ) ;
#8368 = CARTESIAN_POINT ( 'NONE',  ( 9.165151389911684987, 40.00000000000000000, -56.36098470834078711 ) ) ;
#8369 = ORIENTED_EDGE ( 'NONE', *, *, #17783, .T. ) ;
#8370 = VECTOR ( 'NONE', #10880, 1000.000000000000000 ) ;
#8371 = CARTESIAN_POINT ( 'NONE',  ( 1.734723475976807094E-14, 20.00000000000000000, -70.71067811865476926 ) ) ;
#8372 = AXIS2_PLACEMENT_3D ( 'NONE', #4392, #22030, #11368 ) ;
#8373 = DIRECTION ( 'NONE',  ( 0.000000000000000000, 0.000000000000000000, 1.000000000000000000 ) ) ;
#8374 = CIRCLE ( 'NONE', #17872, 0.9999999999999974465 ) ;
#8375 = EDGE_LOOP ( 'NONE', ( #8628, #21847, #1497, #11638 ) ) ;
#8376 = VERTEX_POINT ( 'NONE', #9163 ) ;
#8377 = APPLICATION_PROTOCOL_DEFINITION ( 'draft international standard', 'automotive_design', 1998, #13389 ) ;
#8378 = VERTEX_POINT ( 'NONE', #19724 ) ;
#8379 = DIRECTION ( 'NONE',  ( 0.000000000000000000, 0.000000000000000000, -1.000000000000000000 ) ) ;
#8380 = CARTESIAN_POINT ( 'NONE',  ( 36.39375341857553536, 7.980461308159658707, -2.999999999999981792 ) ) ;
#8381 = CARTESIAN_POINT ( 'NONE',  ( 30.33632613426184932, -11.35354668330706929, -2.999999999999971578 ) ) ;
#8382 = CYLINDRICAL_SURFACE ( 'NONE', #17110, 16.49999999999999645 ) ;
#8383 = CARTESIAN_POINT ( 'NONE',  ( 12.24744603029285273, 40.00000000000000000, 54.43639671998466412 ) ) ;
#8384 = VERTEX_POINT ( 'NONE', #10994 ) ;
#8385 = DIRECTION ( 'NONE',  ( -0.7071067811865561215, 0.000000000000000000, -0.7071067811865390240 ) ) ;
#8387 = AXIS2_PLACEMENT_3D ( 'NONE', #604, #12503, #19516 ) ;
#8386 = DIRECTION ( 'NONE',  ( -1.000000000000000000, 0.000000000000000000, 0.000000000000000000 ) ) ;
#8388 = ORIENTED_EDGE ( 'NONE', *, *, #18322, .T. ) ;
#8389 = CARTESIAN_POINT ( 'NONE',  ( 32.14641817400190860, 18.83615802559793195, 2.999999999999995559 ) ) ;
#8390 = EDGE_CURVE ( 'NONE', #6061, #9986, #16087, .T. ) ;
#8391 = DIRECTION ( 'NONE',  ( 0.000000000000000000, -1.000000000000000000, 0.000000000000000000 ) ) ;
#8392 = DIRECTION ( 'NONE',  ( -0.000000000000000000, 1.000000000000000000, -0.000000000000000000 ) ) ;
#8393 = ORIENTED_EDGE ( 'NONE', *, *, #4213, .F. ) ;
#8394 = CARTESIAN_POINT ( 'NONE',  ( -0.7351298805842383377, 39.99998559474256865, -49.30628110933329822 ) ) ;
#8395 = ORIENTED_EDGE ( 'NONE', *, *, #4776, .F. ) ;
#8396 = FACE_OUTER_BOUND ( 'NONE', #7953, .T. ) ;
#8397 = CARTESIAN_POINT ( 'NONE',  ( -14.95260096911754566, 3.243207204902324392, 56.55590526898573955 ) ) ;
#8398 = VERTEX_POINT ( 'NONE', #9400 ) ;
#8399 = CARTESIAN_POINT ( 'NONE',  ( -34.99999999999999289, 40.00000000000000000, 58.99999999999995737 ) ) ;
#8400 = EDGE_CURVE ( 'NONE', #16662, #22210, #4, .T. ) ;
#8401 = CARTESIAN_POINT ( 'NONE',  ( 35.00000000000058265, 40.00000000000000711, -52.47500000000076170 ) ) ;
#8402 = CARTESIAN_POINT ( 'NONE',  ( 42.50000000000000711, -5.000000000000000000, 49.60000000000000853 ) ) ;
#8403 = CARTESIAN_POINT ( 'NONE',  ( 17.96553007763552401, 11.19640018279076976, -57.57421575614285558 ) ) ;
#8404 = CIRCLE ( 'NONE', #8028, 2.500000000000008882 ) ;
#8405 = VERTEX_POINT ( 'NONE', #693 ) ;
#8406 = ORIENTED_EDGE ( 'NONE', *, *, #3162, .F. ) ;
#8407 = ORIENTED_EDGE ( 'NONE', *, *, #2380, .T. ) ;
#8408 = DIRECTION ( 'NONE',  ( 1.296372316667914327E-16, 1.000000000000000000, -0.000000000000000000 ) ) ;
#8409 = ORIENTED_EDGE ( 'NONE', *, *, #3449, .F. ) ;
#8410 = CARTESIAN_POINT ( 'NONE',  ( -2.999964809119741727, 22.19870380085767891, 6.485293816093604669 ) ) ;
#8411 = LINE ( 'NONE', #22400, #11848 ) ;
#8412 = EDGE_CURVE ( 'NONE', #16827, #12526, #13887, .T. ) ;
#8413 = AXIS2_PLACEMENT_3D ( 'NONE', #19483, #3787, #16032 ) ;
#8414 = FACE_OUTER_BOUND ( 'NONE', #596, .T. ) ;
#8415 = ORIENTED_EDGE ( 'NONE', *, *, #19133, .T. ) ;
#8416 = FACE_OUTER_BOUND ( 'NONE', #16962, .T. ) ;
#8417 = CARTESIAN_POINT ( 'NONE',  ( -2.999999999999999112, 16.00000000000000000, 6.485281374238567764 ) ) ;
#8418 = ORIENTED_EDGE ( 'NONE', *, *, #1897, .F. ) ;
#8419 = CARTESIAN_POINT ( 'NONE',  ( 12.82970538955508566, 1.687462484002703267, 55.75926248610235803 ) ) ;
#8420 = AXIS2_PLACEMENT_3D ( 'NONE', #17261, #11062, #12778 ) ;
#8421 = VERTEX_POINT ( 'NONE', #801 ) ;
#8422 = CYLINDRICAL_SURFACE ( 'NONE', #15932, 19.11328065563151668 ) ;
#8423 = DIRECTION ( 'NONE',  ( 0.000000000000000000, 0.000000000000000000, 1.000000000000000000 ) ) ;
#8424 = DIRECTION ( 'NONE',  ( 0.000000000000000000, 1.000000000000000000, 0.000000000000000000 ) ) ;
#8425 = CARTESIAN_POINT ( 'NONE',  ( -8.492273200209872641, 39.51732067042856045, 54.09038547598553492 ) ) ;
#8426 = FACE_OUTER_BOUND ( 'NONE', #10002, .T. ) ;
#8427 = AXIS2_PLACEMENT_3D ( 'NONE', #1243, #17388, #6631 ) ;
#8428 = DIRECTION ( 'NONE',  ( 6.505213034913038160E-19, 3.903127820947822896E-18, 1.000000000000000000 ) ) ;
#8430 = ORIENTED_EDGE ( 'NONE', *, *, #18143, .F. ) ;
#8429 = ADVANCED_FACE ( 'NONE', ( #4244 ), #9733, .F. ) ;
#8431 = PRODUCT_RELATED_PRODUCT_CATEGORY ( 'part', '', ( #10941 ) ) ;
#8432 = ORIENTED_EDGE ( 'NONE', *, *, #13669, .F. ) ;
#8433 = ORIENTED_EDGE ( 'NONE', *, *, #12806, .F. ) ;
#8434 = EDGE_LOOP ( 'NONE', ( #18614, #9584, #8246, #18274, #5149 ) ) ;
#8435 = CARTESIAN_POINT ( 'NONE',  ( -12.37316313323532491, 4.263667856436507364, 58.19925355777651532 ) ) ;
#8436 = EDGE_CURVE ( 'NONE', #12666, #13122, #18669, .T. ) ;
#8437 = CYLINDRICAL_SURFACE ( 'NONE', #11806, 2.499999999999995115 ) ;
#8438 = CARTESIAN_POINT ( 'NONE',  ( 2.243244216241373046, 39.96968658937159091, -50.39827808307496326 ) ) ;
#8439 = CARTESIAN_POINT ( 'NONE',  ( -41.39271818392636959, 7.000000000000000000, -5.943569790512535533 ) ) ;
#8440 = CARTESIAN_POINT ( 'NONE',  ( 9.689843208404433028, 39.33333333333334991, 54.54983754392749518 ) ) ;
#8441 = CIRCLE ( 'NONE', #13905, 2.499999999999998668 ) ;
#8442 = SHAPE_REPRESENTATION ( 'MAS-345', ( #12764, #9849, #13120, #14949, #1431, #2916, #3273, #11302, #14209, #20836, #19003, #2546 ), #20099 ) ;
#8443 = VERTEX_POINT ( 'NONE', #11217 ) ;
#8444 = DIRECTION ( 'NONE',  ( 6.505213034913038160E-19, 3.903127820947822896E-18, 1.000000000000000000 ) ) ;
#8445 = CARTESIAN_POINT ( 'NONE',  ( -6.607276061855908544, 39.99999999999999289, -52.37472751582438946 ) ) ;
#8446 = CARTESIAN_POINT ( 'NONE',  ( -10.00000000000000000, -4.824555320336763486, 3.000000000000000000 ) ) ;
#8447 = CARTESIAN_POINT ( 'NONE',  ( -27.64365646977275048, -17.09029715894938661, -6.999999999999950262 ) ) ;
#8448 = EDGE_CURVE ( 'NONE', #8987, #11042, #7784, .T. ) ;
#8449 = VERTEX_POINT ( 'NONE', #13254 ) ;
#8450 = CARTESIAN_POINT ( 'NONE',  ( 42.50000000000000711, -9.600000000000001421, 47.50000000000000711 ) ) ;
#8451 = ORIENTED_EDGE ( 'NONE', *, *, #17139, .F. ) ;
#8452 = CARTESIAN_POINT ( 'NONE',  ( -36.76383501243532947, -2.502446443229913594E-13, -6.859353255829918616 ) ) ;
#8453 = DIRECTION ( 'NONE',  ( 8.659560562354634570E-17, 0.7071067811865721087, -0.7071067811865230368 ) ) ;
#8454 = CARTESIAN_POINT ( 'NONE',  ( -1.583519045122685265, -4.618580011808625763, -46.65783332780171833 ) ) ;
#8455 = DIRECTION ( 'NONE',  ( -0.000000000000000000, -1.000000000000000000, -0.000000000000000000 ) ) ;
#8456 = ADVANCED_FACE ( 'NONE', ( #7675 ), #10362, .T. ) ;
#8457 = ADVANCED_FACE ( 'NONE', ( #5953 ), #18436, .T. ) ;
#8458 = ORIENTED_EDGE ( 'NONE', *, *, #5450, .T. ) ;
#8459 = VECTOR ( 'NONE', #5877, 1000.000000000000000 ) ;
#8460 = ORIENTED_EDGE ( 'NONE', *, *, #21500, .F. ) ;
#8461 = DIRECTION ( 'NONE',  ( -1.000000000000000000, 0.000000000000000000, 0.000000000000000000 ) ) ;
#8462 = EDGE_LOOP ( 'NONE', ( #16718, #18801 ) ) ;
#8463 = CARTESIAN_POINT ( 'NONE',  ( 11.84669267190939124, 10.76938159504117110, 44.31876460048056998 ) ) ;
#8464 = AXIS2_PLACEMENT_3D ( 'NONE', #3231, #22481, #8596 ) ;
#8465 = CYLINDRICAL_SURFACE ( 'NONE', #1205, 2.500000000000002220 ) ;
#8466 = DIRECTION ( 'NONE',  ( 0.000000000000000000, 0.000000000000000000, -1.000000000000000000 ) ) ;
#8467 = CARTESIAN_POINT ( 'NONE',  ( -18.13678767553130200, 6.731837175185868105, -57.58481432322442117 ) ) ;
#8468 = CARTESIAN_POINT ( 'NONE',  ( -3.803763136379629373, 39.91204990968978450, 51.45951558227579170 ) ) ;
#8469 = CARTESIAN_POINT ( 'NONE',  ( -10.58465497539836342, 37.06540556999310354, 54.84139108225201653 ) ) ;
#8470 = EDGE_CURVE ( 'NONE', #17781, #14951, #14624, .T. ) ;
#8471 = ORIENTED_EDGE ( 'NONE', *, *, #12725, .T. ) ;
#8472 = CARTESIAN_POINT ( 'NONE',  ( 11.37797799463863768, 29.78145794493465104, 44.06891764425670743 ) ) ;
#8473 =( NAMED_UNIT ( * ) SI_UNIT ( $, .STERADIAN. ) SOLID_ANGLE_UNIT ( ) );
#8474 = DIRECTION ( 'NONE',  ( -1.000000000000000000, 0.000000000000000000, 0.000000000000000000 ) ) ;
#8475 = CARTESIAN_POINT ( 'NONE',  ( 35.91964150878187922, 4.104665049622501449, -2.933296326616344984 ) ) ;
#8476 = ORIENTED_EDGE ( 'NONE', *, *, #10524, .T. ) ;
#8477 = DIRECTION ( 'NONE',  ( -1.000000000000000000, -9.002681209562840861E-16, 0.000000000000000000 ) ) ;
#8478 = DIRECTION ( 'NONE',  ( -0.000000000000000000, -1.000000000000000000, -0.000000000000000000 ) ) ;
#8479 = EDGE_CURVE ( 'NONE', #14915, #20230, #7692, .T. ) ;
#8480 = ADVANCED_FACE ( 'NONE', ( #18326 ), #2643, .T. ) ;
#8481 = AXIS2_PLACEMENT_3D ( 'NONE', #8518, #6693, #13772 ) ;
#8482 = ORIENTED_EDGE ( 'NONE', *, *, #7041, .T. ) ;
#8483 = EDGE_CURVE ( 'NONE', #9582, #4303, #20499, .T. ) ;
#8484 = ORIENTED_EDGE ( 'NONE', *, *, #17041, .F. ) ;
#8485 = CARTESIAN_POINT ( 'NONE',  ( 20.17230487860821597, 25.34312177887337825, -6.999999999999950262 ) ) ;
#8486 = LINE ( 'NONE', #1844, #12128 ) ;
#8487 = DIRECTION ( 'NONE',  ( 0.000000000000000000, 0.000000000000000000, 1.000000000000000000 ) ) ;
#8488 = DIRECTION ( 'NONE',  ( 1.000000000000000000, 1.208970125616067650E-17, 0.000000000000000000 ) ) ;
#8489 = DIRECTION ( 'NONE',  ( -0.000000000000000000, -0.000000000000000000, -1.000000000000000000 ) ) ;
#8490 = ORIENTED_EDGE ( 'NONE', *, *, #645, .F. ) ;
#8491 = LINE ( 'NONE', #10309, #19354 ) ;
#8492 = CARTESIAN_POINT ( 'NONE',  ( -12.24744603029287937, 40.00000000000000000, -54.43639671998464991 ) ) ;
#8493 = EDGE_LOOP ( 'NONE', ( #10447, #9149, #2102, #8294 ) ) ;
#8494 = CARTESIAN_POINT ( 'NONE',  ( 1.583519045122702806, -4.618580011808624874, -46.65783332780173964 ) ) ;
#8495 = DIRECTION ( 'NONE',  ( 6.505213034913038160E-19, 3.903127820947822896E-18, 1.000000000000000000 ) ) ;
#8496 = AXIS2_PLACEMENT_3D ( 'NONE', #3799, #9408, #21212 ) ;
#8497 = CARTESIAN_POINT ( 'NONE',  ( -42.50000000000000711, -5.000000000000000000, 47.50000000000000711 ) ) ;
#8498 = CARTESIAN_POINT ( 'NONE',  ( 6.217946977017707155, 39.75326280521958466, 52.92450750590739261 ) ) ;
#8499 = ORIENTED_EDGE ( 'NONE', *, *, #3068, .F. ) ;
#8500 = CARTESIAN_POINT ( 'NONE',  ( -1.485224345418334257, 39.99052334577585555, -49.86416394167165578 ) ) ;
#8501 = EDGE_CURVE ( 'NONE', #7531, #14915, #20, .T. ) ;
#8502 = ORIENTED_EDGE ( 'NONE', *, *, #5444, .T. ) ;
#8503 = CARTESIAN_POINT ( 'NONE',  ( 5.551115123125782702E-14, -1.387778780781445676E-13, -5.749999999999949374 ) ) ;
#8504 = CARTESIAN_POINT ( 'NONE',  ( -15.34956869069049823, 36.37910824616915306, 56.69201590313574712 ) ) ;
#8505 = ORIENTED_EDGE ( 'NONE', *, *, #6388, .T. ) ;
#8506 = CARTESIAN_POINT ( 'NONE',  ( -6.000000000000000888, -40.00000000000000000, -5.999999999999998224 ) ) ;
#8507 = CYLINDRICAL_SURFACE ( 'NONE', #553, 50.00000000000001421 ) ;
#8508 = CARTESIAN_POINT ( 'NONE',  ( -42.50000000000000711, -5.000000000000000000, -47.50000000000000000 ) ) ;
#8510 = ADVANCED_FACE ( 'NONE', ( #16839 ), #12814, .T. ) ;
#8509 = VERTEX_POINT ( 'NONE', #11102 ) ;
#8511 = VECTOR ( 'NONE', #21521, 1000.000000000000000 ) ;
#8512 = CIRCLE ( 'NONE', #17648, 3.399999999999995470 ) ;
#8513 = EDGE_CURVE ( 'NONE', #4381, #20633, #22229, .T. ) ;
#8514 = ORIENTED_EDGE ( 'NONE', *, *, #5270, .F. ) ;
#8515 = EDGE_LOOP ( 'NONE', ( #3001, #5105, #11849, #3097 ) ) ;
#8516 = DIRECTION ( 'NONE',  ( -1.000000000000000000, 0.000000000000000000, 0.000000000000000000 ) ) ;
#8517 = ORIENTED_EDGE ( 'NONE', *, *, #12635, .F. ) ;
#8518 = CARTESIAN_POINT ( 'NONE',  ( -3.656418565264246467, -37.07861450834820971, 2.999999999999995559 ) ) ;
#8519 = CARTESIAN_POINT ( 'NONE',  ( 21.21578383525635658, 27.34973130705544619, 58.39578210113617729 ) ) ;
#8520 = CARTESIAN_POINT ( 'NONE',  ( -42.50000000000000711, -5.000000000000000000, 47.50000000000000711 ) ) ;
#8521 = EDGE_CURVE ( 'NONE', #14798, #7317, #3965, .T. ) ;
#8522 = ORIENTED_EDGE ( 'NONE', *, *, #11352, .T. ) ;
#8523 = CARTESIAN_POINT ( 'NONE',  ( 28.88846368933348074, 19.59430950039314823, 2.999999999999995559 ) ) ;
#8524 = DIRECTION ( 'NONE',  ( -0.000000000000000000, -0.000000000000000000, -1.000000000000000000 ) ) ;
#8525 = VERTEX_POINT ( 'NONE', #9949 ) ;
#8526 = DIRECTION ( 'NONE',  ( 1.000000000000000000, 0.000000000000000000, 0.000000000000000000 ) ) ;
#8527 = DIRECTION ( 'NONE',  ( -0.000000000000000000, -1.000000000000000000, -0.000000000000000000 ) ) ;
#8528 = ORIENTED_EDGE ( 'NONE', *, *, #3197, .T. ) ;
#8529 = CARTESIAN_POINT ( 'NONE',  ( -31.11077005834421527, 4.936596639065232495, -2.999999999999971578 ) ) ;
#8530 = DIRECTION ( 'NONE',  ( 0.000000000000000000, 0.000000000000000000, -1.000000000000000000 ) ) ;
#8531 = CARTESIAN_POINT ( 'NONE',  ( 4.238639668822796917E-15, 4.500000000000007105, 0.000000000000000000 ) ) ;
#8532 = DIRECTION ( 'NONE',  ( 6.505213034913038160E-19, 3.903127820947822896E-18, 1.000000000000000000 ) ) ;
#8533 = TOROIDAL_SURFACE ( 'NONE', #4881, 34.90673715956759082, 8.750000000000000000 ) ;
#8534 = CARTESIAN_POINT ( 'NONE',  ( -31.88709182564695865, 6.070730550690822902, -7.000000000000006217 ) ) ;
#8535 = AXIS2_PLACEMENT_3D ( 'NONE', #9445, #15960, #10801 ) ;
#8536 = EDGE_CURVE ( 'NONE', #8959, #12838, #9899, .T. ) ;
#8537 = FACE_OUTER_BOUND ( 'NONE', #17106, .T. ) ;
#8538 = ORIENTED_EDGE ( 'NONE', *, *, #10471, .F. ) ;
#8539 = EDGE_LOOP ( 'NONE', ( #6548, #3007, #17882, #15033 ) ) ;
#8540 = ORIENTED_EDGE ( 'NONE', *, *, #5450, .F. ) ;
#8541 = ORIENTED_EDGE ( 'NONE', *, *, #18556, .T. ) ;
#8542 = CARTESIAN_POINT ( 'NONE',  ( -4.025500340002485800, 36.54278193890309012, 2.800654218530485018 ) ) ;
#8543 = CARTESIAN_POINT ( 'NONE',  ( -23.74488952252751162, 25.58633464742629471, -2.999999999999971578 ) ) ;
#8544 = AXIS2_PLACEMENT_3D ( 'NONE', #13773, #17108, #3606 ) ;
#8545 = AXIS2_PLACEMENT_3D ( 'NONE', #17283, #13946, #15561 ) ;
#8546 = LINE ( 'NONE', #6956, #18623 ) ;
#8547 = DIRECTION ( 'NONE',  ( -0.000000000000000000, 1.000000000000000000, -0.000000000000000000 ) ) ;
#8548 = CARTESIAN_POINT ( 'NONE',  ( 5.466611488789254736, 39.81233002189807024, 52.49274978756180587 ) ) ;
#8549 = AXIS2_PLACEMENT_3D ( 'NONE', #5277, #15565, #13502 ) ;
#8550 = ORIENTED_EDGE ( 'NONE', *, *, #15860, .T. ) ;
#8551 = CARTESIAN_POINT ( 'NONE',  ( 19.99999999999999645, 1.500000000000009104, 2.449293598294705724E-15 ) ) ;
#8552 = CARTESIAN_POINT ( 'NONE',  ( -2.175117848631995532, 40.00000000000000711, -50.07592579258850662 ) ) ;
#8553 = CYLINDRICAL_SURFACE ( 'NONE', #6513, 31.50000000000001421 ) ;
#8554 = CARTESIAN_POINT ( 'NONE',  ( 10.34137811700762555, 39.99999999999997868, -53.75702834151196896 ) ) ;
#8555 = CARTESIAN_POINT ( 'NONE',  ( 4.898587196589410857E-16, 29.97499999999999787, -3.999999999999998224 ) ) ;
#8556 = ADVANCED_FACE ( 'NONE', ( #15324 ), #6525, .T. ) ;
#8557 = AXIS2_PLACEMENT_3D ( 'NONE', #7180, #14265, #5145 ) ;
#8558 = ORIENTED_EDGE ( 'NONE', *, *, #13729, .F. ) ;
#8559 = CARTESIAN_POINT ( 'NONE',  ( 21.65063509461118230, 12.49999999999984368, -2.999999999999988898 ) ) ;
#8560 = CARTESIAN_POINT ( 'NONE',  ( -14.31751149541525336, 33.97259629115305302, 58.93694582298957840 ) ) ;
#8561 = ADVANCED_FACE ( 'NONE', ( #5156 ), #6408, .F. ) ;
#8562 = EDGE_LOOP ( 'NONE', ( #5520, #15057, #23, #1238, #20563, #17188 ) ) ;
#8563 = ADVANCED_FACE ( 'NONE', ( #22345 ), #4703, .T. ) ;
#8564 = VECTOR ( 'NONE', #16370, 1000.000000000000000 ) ;
#8565 = CYLINDRICAL_SURFACE ( 'NONE', #9337, 2.500000000000002220 ) ;
#8566 = DIRECTION ( 'NONE',  ( -1.000000000000000000, 0.000000000000000000, 0.000000000000000000 ) ) ;
#8567 = CARTESIAN_POINT ( 'NONE',  ( -2.109039589833474171, 34.88603667777789497, 38.90259428073981240 ) ) ;
#8568 = VERTEX_POINT ( 'NONE', #15548 ) ;
#8569 = ORIENTED_EDGE ( 'NONE', *, *, #2239, .F. ) ;
#8570 = FACE_OUTER_BOUND ( 'NONE', #894, .T. ) ;
#8571 = EDGE_CURVE ( 'NONE', #10113, #2931, #21232, .T. ) ;
#8572 = CIRCLE ( 'NONE', #15880, 2.499999999999995115 ) ;
#8573 = CARTESIAN_POINT ( 'NONE',  ( 16.99647590252675755, 30.48934413892762052, 3.000000000000019984 ) ) ;
#8574 = VERTEX_POINT ( 'NONE', #12127 ) ;
#8575 = CARTESIAN_POINT ( 'NONE',  ( 14.99999999999998934, 19.22713695939442857, 45.82575694955839651 ) ) ;
#8576 = CARTESIAN_POINT ( 'NONE',  ( 8.331955809010596070, 38.18181818181818699, -56.36098470834070895 ) ) ;
#8577 = DIRECTION ( 'NONE',  ( 0.000000000000000000, 0.000000000000000000, -1.000000000000000000 ) ) ;
#8578 = EDGE_CURVE ( 'NONE', #5921, #14950, #20144, .T. ) ;
#8579 = CARTESIAN_POINT ( 'NONE',  ( -19.65511384563465569, 23.80142929986424960, -60.53962097676930654 ) ) ;
#8580 = AXIS2_PLACEMENT_3D ( 'NONE', #18825, #18938, #1521 ) ;
#8581 = CARTESIAN_POINT ( 'NONE',  ( 19.99999999999999645, -4.500000000000013323, 0.000000000000000000 ) ) ;
#8582 = EDGE_LOOP ( 'NONE', ( #1464, #12970, #11471, #972 ) ) ;
#8583 = PLANE ( 'NONE',  #17085 ) ;
#8584 = SURFACE_SIDE_STYLE ('',( #1833 ) ) ;
#8585 = FACE_BOUND ( 'NONE', #6610, .T. ) ;
#8586 = CARTESIAN_POINT ( 'NONE',  ( -30.00000000000001421, 20.00000000000000711, -100.0000000000000000 ) ) ;
#8587 = ORIENTED_EDGE ( 'NONE', *, *, #14762, .F. ) ;
#8588 = CARTESIAN_POINT ( 'NONE',  ( 3.330669073875469621E-13, -1.110223024625156540E-13, -2.999999999999971578 ) ) ;
#8589 = CIRCLE ( 'NONE', #21034, 1.000000000000000888 ) ;
#8590 = ORIENTED_EDGE ( 'NONE', *, *, #15224, .T. ) ;
#8591 = ADVANCED_FACE ( 'NONE', ( #10390 ), #8355, .T. ) ;
#8592 = APPLICATION_PROTOCOL_DEFINITION ( 'draft international standard', 'automotive_design', 1998, #22052 ) ;
#8593 = CIRCLE ( 'NONE', #22161, 19.11328065563152379 ) ;
#8594 = ORIENTED_EDGE ( 'NONE', *, *, #13992, .F. ) ;
#8595 = DIRECTION ( 'NONE',  ( -0.000000000000000000, -0.000000000000000000, -1.000000000000000000 ) ) ;
#8596 = DIRECTION ( 'NONE',  ( -1.000000000000000000, -1.208970125616014957E-17, 0.000000000000000000 ) ) ;
#8597 = CIRCLE ( 'NONE', #3505, 1.000000000000000888 ) ;
#8598 = CARTESIAN_POINT ( 'NONE',  ( -24.03323817228468329, 20.36304159388335933, 3.000000000000009770 ) ) ;
#8599 = CARTESIAN_POINT ( 'NONE',  ( -34.99999999999999289, 0.000000000000000000, -3.012171160963566127E-14 ) ) ;
#8600 = CARTESIAN_POINT ( 'NONE',  ( 3.330669073875469621E-13, -1.110223024625156540E-13, -2.999999999999971578 ) ) ;
#8601 = ORIENTED_EDGE ( 'NONE', *, *, #5813, .T. ) ;
#8602 = CARTESIAN_POINT ( 'NONE',  ( 35.00000000000000000, 25.00000000000000000, -16.99999999999997868 ) ) ;
#8603 = CARTESIAN_POINT ( 'NONE',  ( -10.06223851446539541, 39.28158160658948361, 54.67678195792279183 ) ) ;
#8604 = ORIENTED_EDGE ( 'NONE', *, *, #3134, .T. ) ;
#8605 = EDGE_CURVE ( 'NONE', #17965, #13528, #13375, .T. ) ;
#8606 = CARTESIAN_POINT ( 'NONE',  ( 29.99999999999998579, 20.00000000000000355, -105.0000000000000142 ) ) ;
#8607 = CARTESIAN_POINT ( 'NONE',  ( 20.10834676944517696, 10.02088872142240383, -58.12296025200761562 ) ) ;
#8608 = AXIS2_PLACEMENT_3D ( 'NONE', #15047, #20349, #4655 ) ;
#8609 = DIRECTION ( 'NONE',  ( 0.000000000000000000, -1.000000000000000000, 0.000000000000000000 ) ) ;
#8610 = CARTESIAN_POINT ( 'NONE',  ( -25.34312177887333561, 20.17230487860788202, -6.999999999999950262 ) ) ;
#8611 = DIRECTION ( 'NONE',  ( 6.505213034913038160E-19, 3.903127820947822896E-18, 1.000000000000000000 ) ) ;
#8612 = VERTEX_POINT ( 'NONE', #13592 ) ;
#8613 = CARTESIAN_POINT ( 'NONE',  ( 42.50000000000000711, -3.738192700042122674, 47.50000000000000711 ) ) ;
#8614 = DIRECTION ( 'NONE',  ( -0.9659258262890680902, -0.2588190451025216832, 1.182917971378669349E-16 ) ) ;
#8615 = ORIENTED_EDGE ( 'NONE', *, *, #9477, .F. ) ;
#8616 = DIRECTION ( 'NONE',  ( -0.000000000000000000, 1.000000000000000000, -0.000000000000000000 ) ) ;
#8617 = CARTESIAN_POINT ( 'NONE',  ( -30.00000000000001421, 20.00000000000000355, 105.0000000000000142 ) ) ;
#8618 = DIRECTION ( 'NONE',  ( 0.000000000000000000, 0.000000000000000000, 1.000000000000000000 ) ) ;
#8619 = CIRCLE ( 'NONE', #12626, 39.00000000000000000 ) ;
#8620 = VECTOR ( 'NONE', #11971, 1000.000000000000000 ) ;
#8621 = FACE_BOUND ( 'NONE', #21554, .T. ) ;
#8622 = ADVANCED_FACE ( 'NONE', ( #20606 ), #5701, .T. ) ;
#8623 = VECTOR ( 'NONE', #10210, 1000.000000000000000 ) ;
#8624 = ORIENTED_EDGE ( 'NONE', *, *, #14974, .F. ) ;
#8625 = VECTOR ( 'NONE', #1910, 1000.000000000000000 ) ;
#8626 = EDGE_LOOP ( 'NONE', ( #8393, #7139, #19765, #5800 ) ) ;
#8627 = ADVANCED_FACE ( 'NONE', ( #10727 ), #3695, .T. ) ;
#8628 = ORIENTED_EDGE ( 'NONE', *, *, #11532, .T. ) ;
#8629 = ORIENTED_EDGE ( 'NONE', *, *, #7865, .T. ) ;
#8630 = DIRECTION ( 'NONE',  ( -1.000000000000000000, 1.275531967630005492E-16, 0.000000000000000000 ) ) ;
#8631 = CARTESIAN_POINT ( 'NONE',  ( 21.43973101033761708, 13.38729130222876762, 58.44776001661261233 ) ) ;
#8632 = CARTESIAN_POINT ( 'NONE',  ( 2.602085213965210642E-15, 5.025303850726727362, 17.00000000000000711 ) ) ;
#8633 = CARTESIAN_POINT ( 'NONE',  ( 8.265432197626479294, 40.00000000000000000, 53.06731919463958747 ) ) ;
#8634 = VERTEX_POINT ( 'NONE', #21400 ) ;
#8635 = CARTESIAN_POINT ( 'NONE',  ( -19.59430950039320152, 28.88846368933331732, -2.999999999999999112 ) ) ;
#8636 = CARTESIAN_POINT ( 'NONE',  ( 90.00000000000000000, 40.00000000000000711, -9.108981535246192915E-16 ) ) ;
#8637 = ORIENTED_EDGE ( 'NONE', *, *, #11796, .F. ) ;
#8638 = AXIS2_PLACEMENT_3D ( 'NONE', #7821, #20201, #16759 ) ;
#8639 = CARTESIAN_POINT ( 'NONE',  ( -6.000920103808232042, -0.8369757414283609531, 52.11565860623115753 ) ) ;
#8640 = VECTOR ( 'NONE', #5912, 1000.000000000000000 ) ;
#8641 = AXIS2_PLACEMENT_3D ( 'NONE', #6940, #19984, #2572 ) ;
#8642 = EDGE_LOOP ( 'NONE', ( #11859, #5521, #10153, #1857 ) ) ;
#8643 = CARTESIAN_POINT ( 'NONE',  ( -19.99999999999999289, -2.799736964075212609E-14, 2.999999999999995559 ) ) ;
#8644 = ORIENTED_EDGE ( 'NONE', *, *, #15453, .T. ) ;
#8645 = CARTESIAN_POINT ( 'NONE',  ( 7.464640338966086475, 38.57205754384674634, -54.30630206323173326 ) ) ;
#8646 = CARTESIAN_POINT ( 'NONE',  ( -1.814315892323006274, 39.98032163334644196, 50.09302599523660149 ) ) ;
#8647 = ADVANCED_FACE ( 'NONE', ( #21290 ), #12559, .T. ) ;
#8648 = CIRCLE ( 'NONE', #21450, 19.11328065563152379 ) ;
#8649 = ADVANCED_FACE ( 'NONE', ( #8807 ), #1475, .T. ) ;
#8650 = CARTESIAN_POINT ( 'NONE',  ( 18.68837533793185912, 7.522086334128933238, 57.74247137455829915 ) ) ;
#8651 = FACE_OUTER_BOUND ( 'NONE', #12505, .T. ) ;
#8652 = DIRECTION ( 'NONE',  ( 0.000000000000000000, 0.000000000000000000, -1.000000000000000000 ) ) ;
#8653 = ADVANCED_FACE ( 'NONE', ( #7079 ), #2208, .T. ) ;
#8654 = AXIS2_PLACEMENT_3D ( 'NONE', #14511, #12347, #88 ) ;
#8655 = AXIS2_PLACEMENT_3D ( 'NONE', #12274, #19280, #238 ) ;
#8656 = ORIENTED_EDGE ( 'NONE', *, *, #22074, .F. ) ;
#8657 = ORIENTED_EDGE ( 'NONE', *, *, #2335, .T. ) ;
#8658 = ORIENTED_EDGE ( 'NONE', *, *, #3893, .T. ) ;
#8659 = VERTEX_POINT ( 'NONE', #5581 ) ;
#8660 = CARTESIAN_POINT ( 'NONE',  ( 2.775557561562891351E-14, -2.775557561562891351E-14, 2.999999999999999112 ) ) ;
#8661 = CIRCLE ( 'NONE', #21846, 4.000000000000000000 ) ;
#8662 = CARTESIAN_POINT ( 'NONE',  ( -13.00000000000011546, 42.51666049839536043, -100.0000000000000000 ) ) ;
#8663 = FACE_OUTER_BOUND ( 'NONE', #14581, .T. ) ;
#8664 = DIRECTION ( 'NONE',  ( -1.000000000000000000, 0.000000000000000000, 0.000000000000000000 ) ) ;
#8665 = CARTESIAN_POINT ( 'NONE',  ( 2.239818980015277017, 39.96978032374031642, 50.39586354373248156 ) ) ;
#8666 = B_SPLINE_CURVE_WITH_KNOTS ( 'NONE', 3,
 ( #5655, #11036, #12630, #18024, #2336, #387, #17808, #16304 ),
 .UNSPECIFIED., .F., .F.,
 ( 4, 2, 2, 4 ),
 ( 0.000000000000000000, 0.002330949112885988446, 0.004661898225771976892, 0.009323796451543943375 ),
 .UNSPECIFIED. ) ;
#8667 = ORIENTED_EDGE ( 'NONE', *, *, #4580, .F. ) ;
#8668 = CARTESIAN_POINT ( 'NONE',  ( 89.99999999999701572, -5.000000000000000000, -5.216535399428728743E-14 ) ) ;
#8669 = CARTESIAN_POINT ( 'NONE',  ( -2.783900127212157738, 40.00000000000000000, -50.42898717388165153 ) ) ;
#8670 = CARTESIAN_POINT ( 'NONE',  ( 3.330669073875469621E-13, -1.110223024625156540E-13, -2.999999999999971578 ) ) ;
#8671 = FACE_OUTER_BOUND ( 'NONE', #20743, .T. ) ;
#8672 = CONICAL_SURFACE ( 'NONE', #4284, 17.00000000000000355, 0.7853981633974539411 ) ;
#8673 = ADVANCED_FACE ( 'NONE', ( #14044, #17731 ), #19238, .F. ) ;
#8674 = ORIENTED_EDGE ( 'NONE', *, *, #8927, .T. ) ;
#8675 = CARTESIAN_POINT ( 'NONE',  ( -13.63965147459812322, 34.63504322468456564, 58.68815147418794709 ) ) ;
#8676 = VERTEX_POINT ( 'NONE', #5259 ) ;
#8677 = FACE_BOUND ( 'NONE', #982, .T. ) ;
#8678 = ADVANCED_FACE ( 'NONE', ( #22694 ), #10848, .T. ) ;
#8679 = DIRECTION ( 'NONE',  ( -1.000000000000000000, 0.000000000000000000, 0.000000000000000000 ) ) ;
#8680 = FACE_OUTER_BOUND ( 'NONE', #15303, .T. ) ;
#8681 = ORIENTED_EDGE ( 'NONE', *, *, #12671, .F. ) ;
#8682 = AXIS2_PLACEMENT_3D ( 'NONE', #8830, #19044, #13962 ) ;
#8683 = VERTEX_POINT ( 'NONE', #10614 ) ;
#8684 = AXIS2_PLACEMENT_3D ( 'NONE', #4951, #19158, #20539 ) ;
#8685 = ADVANCED_FACE ( 'NONE', ( #5368, #13937 ), #15671, .F. ) ;
#8686 = VERTEX_POINT ( 'NONE', #1926 ) ;
#8687 = CARTESIAN_POINT ( 'NONE',  ( -7.463862311150981199, -35.99819890246952525, 2.800654218530485018 ) ) ;
#8688 = CARTESIAN_POINT ( 'NONE',  ( 35.00000000000000000, -4.928932188134504955, 4.258610482196280173E-15 ) ) ;
#8689 = VERTEX_POINT ( 'NONE', #3663 ) ;
#8690 = ADVANCED_FACE ( 'NONE', ( #12234 ), #3322, .T. ) ;
#8691 = DIRECTION ( 'NONE',  ( 1.000000000000000000, 0.000000000000000000, 0.000000000000000000 ) ) ;
#8692 = AXIS2_PLACEMENT_3D ( 'NONE', #6791, #12061, #11945 ) ;
#8693 = AXIS2_PLACEMENT_3D ( 'NONE', #15985, #9549, #1807 ) ;
#8694 = DIRECTION ( 'NONE',  ( -0.000000000000000000, -1.000000000000000000, -0.000000000000000000 ) ) ;
#8695 = CARTESIAN_POINT ( 'NONE',  ( -27.01645732367843777, -17.86915608785696818, -6.999999999999950262 ) ) ;
#8696 = CARTESIAN_POINT ( 'NONE',  ( -19.81381843823601585, 22.85613052104876530, -58.09821304537217657 ) ) ;
#8697 = CARTESIAN_POINT ( 'NONE',  ( -30.07487443287963558, 12.31876324338265860, -6.999999999999950262 ) ) ;
#8698 = AXIS2_PLACEMENT_3D ( 'NONE', #5371, #21522, #12791 ) ;
#8699 = ORIENTED_EDGE ( 'NONE', *, *, #17157, .T. ) ;
#8700 = DIRECTION ( 'NONE',  ( -0.000000000000000000, -0.000000000000000000, 1.000000000000000000 ) ) ;
#8701 = VECTOR ( 'NONE', #14278, 1000.000000000000114 ) ;
#8702 = DIRECTION ( 'NONE',  ( -0.000000000000000000, 1.000000000000000000, -0.000000000000000000 ) ) ;
#8703 = CARTESIAN_POINT ( 'NONE',  ( 36.54278193890314697, 4.025500340002402311, -2.800654218530457484 ) ) ;
#8704 = AXIS2_PLACEMENT_3D ( 'NONE', #3997, #12789, #19801 ) ;
#8705 = ORIENTED_EDGE ( 'NONE', *, *, #13539, .T. ) ;
#8706 = DIRECTION ( 'NONE',  ( 3.585095183685401065E-15, 0.000000000000000000, -1.000000000000000000 ) ) ;
#8707 = CARTESIAN_POINT ( 'NONE',  ( 14.93538271375424742, 34.13396246814559731, -2.999999999999999112 ) ) ;
#8708 = CIRCLE ( 'NONE', #22271, 1.000000000000000888 ) ;
#8709 = EDGE_CURVE ( 'NONE', #12493, #18822, #11728, .T. ) ;
#8710 = ORIENTED_EDGE ( 'NONE', *, *, #21309, .F. ) ;
#8711 = AXIS2_PLACEMENT_3D ( 'NONE', #12297, #17226, #19301 ) ;
#8712 = VECTOR ( 'NONE', #17275, 1000.000000000000114 ) ;
#8713 = AXIS2_PLACEMENT_3D ( 'NONE', #4092, #21729, #2368 ) ;
#8714 = AXIS2_PLACEMENT_3D ( 'NONE', #8785, #20932, #5345 ) ;
#8715 = ORIENTED_EDGE ( 'NONE', *, *, #15859, .F. ) ;
#8716 = FACE_OUTER_BOUND ( 'NONE', #3917, .T. ) ;
#8717 = EDGE_CURVE ( 'NONE', #4617, #3722, #7703, .T. ) ;
#8718 = CARTESIAN_POINT ( 'NONE',  ( 5.770190843040702511, -4.767707482267821817, 49.21533144469336918 ) ) ;
#8719 = CARTESIAN_POINT ( 'NONE',  ( 34.99999999999999289, -5.000000000000000000, -54.99999999999705835 ) ) ;
#8720 = FACE_OUTER_BOUND ( 'NONE', #7777, .T. ) ;
#8721 = EDGE_LOOP ( 'NONE', ( #6080, #17614 ) ) ;
#8722 = CARTESIAN_POINT ( 'NONE',  ( 0.000000000000000000, 30.00000000000000000, -8.999999999999998224 ) ) ;
#8723 = CARTESIAN_POINT ( 'NONE',  ( -11.06593724743309082, 39.99999999999999289, -53.99256019164670306 ) ) ;
#8724 = EDGE_LOOP ( 'NONE', ( #5307, #3708, #9296, #7828 ) ) ;
#8725 = CARTESIAN_POINT ( 'NONE',  ( 0.7809641287214669214, -4.625293788890100011, -46.06432795380058565 ) ) ;
#8726 = CARTESIAN_POINT ( 'NONE',  ( 19.73349596156085184, 30.70641346160533303, -58.02568834892367988 ) ) ;
#8727 =( REPRESENTATION_RELATIONSHIP ('NONE','NONE', #8442, #6502 ) REPRESENTATION_RELATIONSHIP_WITH_TRANSFORMATION ( #4730 )SHAPE_REPRESENTATION_RELATIONSHIP( ) );
#8728 = CARTESIAN_POINT ( 'NONE',  ( 17.99999999999998579, 20.00000000000000355, 103.0000000000000284 ) ) ;
#8729 = CARTESIAN_POINT ( 'NONE',  ( 2.220446049250313081E-13, -8.326672684688674053E-14, 2.800654218530498785 ) ) ;
#8730 = CARTESIAN_POINT ( 'NONE',  ( 3.330669073875469621E-13, -1.110223024625156540E-13, -2.999999999999971578 ) ) ;
#8731 = CIRCLE ( 'NONE', #14569, 11.99999999999985434 ) ;
#8732 = ORIENTED_EDGE ( 'NONE', *, *, #20815, .F. ) ;
#8733 = DIRECTION ( 'NONE',  ( -0.000000000000000000, -0.000000000000000000, 1.000000000000000000 ) ) ;
#8734 = CIRCLE ( 'NONE', #21541, 2.500000000000002220 ) ;
#8735 = CARTESIAN_POINT ( 'NONE',  ( -34.00000000000000000, -6.180736333215561373, 4.163799117101000559E-15 ) ) ;
#8736 = AXIS2_PLACEMENT_3D ( 'NONE', #3852, #3974, #7738 ) ;
#8737 = VERTEX_POINT ( 'NONE', #14160 ) ;
#8738 = CARTESIAN_POINT ( 'NONE',  ( 28.49999999999998224, 19.99999999999999645, 105.0000000000000142 ) ) ;
#8739 = AXIS2_PLACEMENT_3D ( 'NONE', #2843, #4216, #9828 ) ;
#8740 = EDGE_CURVE ( 'NONE', #2277, #2772, #11354, .T. ) ;
#8741 = CARTESIAN_POINT ( 'NONE',  ( -28.52469787935786982, 7.000000000000000000, -4.095854054471906203 ) ) ;
#8742 = CARTESIAN_POINT ( 'NONE',  ( 42.50000000000000711, -12.00000000000012434, -44.97499999999988773 ) ) ;
#8743 = VECTOR ( 'NONE', #345, 1000.000000000000000 ) ;
#8744 = B_SPLINE_SURFACE_WITH_KNOTS ( 'NONE', 1, 3, ( 
 ( #1568, #11763, #6964, #13923, #8554, #22552 ),
 ( #18760, #20590, #17031, #4900, #20831, #12109 ) ),
 .UNSPECIFIED., .F., .F., .F.,
 ( 2, 2 ),
 ( 4, 2, 4 ),
 ( 0.000000000000000000, 1.000000000000000000 ),
 ( 0.000000000000000000, 0.001214050925806519710, 0.002428101851613039420 ),
 .UNSPECIFIED. ) ;
#8745 = EDGE_CURVE ( 'NONE', #8887, #21941, #14274, .T. ) ;
#8746 = EDGE_CURVE ( 'NONE', #3679, #14442, #15046, .T. ) ;
#8747 = VERTEX_POINT ( 'NONE', #6253 ) ;
#8748 = ORIENTED_EDGE ( 'NONE', *, *, #8361, .T. ) ;
#8749=STYLED_ITEM('',(#22741),#17806);
#8750 = EDGE_LOOP ( 'NONE', ( #953, #21327, #8799, #7473 ) ) ;
#8751 = AXIS2_PLACEMENT_3D ( 'NONE', #19415, #17673, #16068 ) ;
#8752 = ORIENTED_EDGE ( 'NONE', *, *, #10684, .T. ) ;
#8753 = LINE ( 'NONE', #19181, #15065 ) ;
#8754 = CARTESIAN_POINT ( 'NONE',  ( 21.56999872847275057, 13.83083564369840701, 58.47776649573041396 ) ) ;
#8755 = CARTESIAN_POINT ( 'NONE',  ( 8.604786169551864816, 40.00000000000000000, 53.19510612370975622 ) ) ;
#8756 = EDGE_LOOP ( 'NONE', ( #21008, #14176, #1357, #5309 ) ) ;
#8757 = CARTESIAN_POINT ( 'NONE',  ( 29.33203831401607786, 20.06142356895397327, 3.000000000000044853 ) ) ;
#8758 = CARTESIAN_POINT ( 'NONE',  ( 1.039655021832692539, -3.147609295952956909, -46.52691668518789214 ) ) ;
#8759 = VERTEX_POINT ( 'NONE', #13211 ) ;
#8760 = AXIS2_PLACEMENT_3D ( 'NONE', #4271, #8151, #9757 ) ;
#8761 = DIRECTION ( 'NONE',  ( 0.000000000000000000, 0.000000000000000000, 1.000000000000000000 ) ) ;
#8762 = EDGE_LOOP ( 'NONE', ( #6974, #21872 ) ) ;
#8763 = DIRECTION ( 'NONE',  ( 0.000000000000000000, -1.000000000000000000, 0.000000000000000000 ) ) ;
#8764 = VERTEX_POINT ( 'NONE', #22063 ) ;
#8765 = CARTESIAN_POINT ( 'NONE',  ( 2.775557561562891351E-14, -2.775557561562891351E-14, 2.999999999999999112 ) ) ;
#8766 = DIRECTION ( 'NONE',  ( 0.000000000000000000, -1.000000000000000000, 0.000000000000000000 ) ) ;
#8767 = CARTESIAN_POINT ( 'NONE',  ( -4.591783869092104453, 39.86870517915106404, 51.95897982375534241 ) ) ;
#8768 = ADVANCED_FACE ( 'NONE', ( #11846 ), #7536, .F. ) ;
#8769 = VECTOR ( 'NONE', #7040, 1000.000000000000000 ) ;
#8770 = B_SPLINE_CURVE_WITH_KNOTS ( 'NONE', 3,
 ( #3110, #17413, #15576, #20635 ),
 .UNSPECIFIED., .F., .F.,
 ( 4, 4 ),
 ( 0.001893031756885503371, 0.003808480026563726851 ),
 .UNSPECIFIED. ) ;
#8771 = CARTESIAN_POINT ( 'NONE',  ( 19.38379237383783149, 24.94684328524480321, 57.98195591854139508 ) ) ;
#8772 = CARTESIAN_POINT ( 'NONE',  ( 25.00000000000000000, -20.00000000000000000, 6.487780019669002523E-15 ) ) ;
#8773 = CARTESIAN_POINT ( 'NONE',  ( 2.602085213965210642E-15, 6.000000000000019540, 0.000000000000000000 ) ) ;
#8774 = ADVANCED_FACE ( 'NONE', ( #20231, #3041 ), #4653, .F. ) ;
#8775 = EDGE_CURVE ( 'NONE', #18499, #5723, #13321, .T. ) ;
#8776 = ORIENTED_EDGE ( 'NONE', *, *, #7634, .T. ) ;
#8777 = ORIENTED_EDGE ( 'NONE', *, *, #13219, .T. ) ;
#8778 = ORIENTED_EDGE ( 'NONE', *, *, #2942, .T. ) ;
#8779 = ADVANCED_FACE ( 'NONE', ( #15157 ), #15677, .T. ) ;
#8780 = EDGE_LOOP ( 'NONE', ( #18041, #12027, #15488, #6244 ) ) ;
#8781 = CARTESIAN_POINT ( 'NONE',  ( 3.330669073875469621E-13, -1.110223024625156540E-13, -2.999999999999971578 ) ) ;
#8782 = DIRECTION ( 'NONE',  ( 0.7071067811865522357, 1.130863789078081945E-17, 0.7071067811865429098 ) ) ;
#8783 = VECTOR ( 'NONE', #5916, 1000.000000000000000 ) ;
#8784 = CARTESIAN_POINT ( 'NONE',  ( -16.66666666666666785, -20.00000000000000000, -23.57022603955158502 ) ) ;
#8785 = CARTESIAN_POINT ( 'NONE',  ( -3.656418565263996889, -37.07861450834837314, -6.999999999999950262 ) ) ;
#8786 = CARTESIAN_POINT ( 'NONE',  ( 2.665759242407653495, 39.95807813352564608, 50.69599102971979221 ) ) ;
#8787 = ORIENTED_EDGE ( 'NONE', *, *, #19065, .F. ) ;
#8788 = DIRECTION ( 'NONE',  ( 6.505213034913038160E-19, 3.903127820947822896E-18, 1.000000000000000000 ) ) ;
#8789 = CARTESIAN_POINT ( 'NONE',  ( -9.272092388914145999, 40.00000000000000000, -53.43088570759663725 ) ) ;
#8790 = DIRECTION ( 'NONE',  ( -0.9659258262890679791, 0.2588190451025219052, 0.000000000000000000 ) ) ;
#8791 = DIRECTION ( 'NONE',  ( -1.000000000000000000, -1.208970125616060717E-17, 0.000000000000000000 ) ) ;
#8792 =( NAMED_UNIT ( * ) PLANE_ANGLE_UNIT ( ) SI_UNIT ( $, .RADIAN. ) );
#8793 = AXIS2_PLACEMENT_3D ( 'NONE', #4472, #912, #9514 ) ;
#8794 = CARTESIAN_POINT ( 'NONE',  ( -19.71583072461107378, 23.39500837205461536, 60.55395521980175033 ) ) ;
#8795 = DIRECTION ( 'NONE',  ( 1.000000000000000000, 0.000000000000000000, 0.000000000000000000 ) ) ;
#8796 = FACE_BOUND ( 'NONE', #21451, .T. ) ;
#8797 = DIRECTION ( 'NONE',  ( 6.505213034913038160E-19, 3.903127820947822896E-18, 1.000000000000000000 ) ) ;
#8798 = DIRECTION ( 'NONE',  ( 0.000000000000000000, 0.7071067811865474617, 0.7071067811865474617 ) ) ;
#8799 = ORIENTED_EDGE ( 'NONE', *, *, #18807, .F. ) ;
#8800 = EDGE_LOOP ( 'NONE', ( #22332, #21258, #3709, #18619 ) ) ;
#8801 = EDGE_CURVE ( 'NONE', #164, #507, #8077, .T. ) ;
#8802 = ORIENTED_EDGE ( 'NONE', *, *, #2128, .T. ) ;
#8803 = DIRECTION ( 'NONE',  ( -0.000000000000000000, 1.000000000000000000, -0.000000000000000000 ) ) ;
#8804 = EDGE_CURVE ( 'NONE', #9999, #20208, #20885, .T. ) ;
#8805 = CYLINDRICAL_SURFACE ( 'NONE', #16385, 2.499999999999998668 ) ;
#8806 = VERTEX_POINT ( 'NONE', #6474 ) ;
#8807 = FACE_OUTER_BOUND ( 'NONE', #11019, .T. ) ;
#8808 = EDGE_CURVE ( 'NONE', #12800, #2882, #18386, .T. ) ;
#8809 = CYLINDRICAL_SURFACE ( 'NONE', #19635, 33.99999999999999289 ) ;
#8810 = DIRECTION ( 'NONE',  ( -1.000000000000000000, 0.000000000000000000, 0.000000000000000000 ) ) ;
#8811 = DIRECTION ( 'NONE',  ( 0.000000000000000000, 1.000000000000000000, 0.000000000000000000 ) ) ;
#8812 = EDGE_LOOP ( 'NONE', ( #14405, #3338, #10665, #1726, #2203, #3603 ) ) ;
#8813 = CARTESIAN_POINT ( 'NONE',  ( -34.99999999999999289, -5.000000000000000000, -3.012171160963566127E-14 ) ) ;
#8814 = CARTESIAN_POINT ( 'NONE',  ( -21.65063509461084834, 12.49999999999965006, 3.000000000000023537 ) ) ;
#8815 = CARTESIAN_POINT ( 'NONE',  ( -90.00000000000000000, 40.00000000000000000, -9.108981535246192915E-16 ) ) ;
#8816 = CARTESIAN_POINT ( 'NONE',  ( -35.00000000000000000, -9.000000000000001776, 1.387778780781445676E-14 ) ) ;
#8817 = VERTEX_POINT ( 'NONE', #8089 ) ;
#8818 = AXIS2_PLACEMENT_3D ( 'NONE', #7846, #3036, #4309 ) ;
#8819 = DIRECTION ( 'NONE',  ( -1.000000000000000000, 1.264902534566421429E-16, 0.000000000000000000 ) ) ;
#8820 = DIRECTION ( 'NONE',  ( 6.505213034913038160E-19, 3.903127820947822896E-18, 1.000000000000000000 ) ) ;
#8821 = EDGE_CURVE ( 'NONE', #6187, #20709, #5508, .T. ) ;
#8822 = ORIENTED_EDGE ( 'NONE', *, *, #7381, .F. ) ;
#8823 = CONTEXT_DEPENDENT_SHAPE_REPRESENTATION ( #526, #6017 ) ;
#8824 = VERTEX_POINT ( 'NONE', #10011 ) ;
#8825 = CARTESIAN_POINT ( 'NONE',  ( 0.6683989176583298164, -3.155640224524286275, 47.80307817979240070 ) ) ;
#8826 = DIRECTION ( 'NONE',  ( 0.000000000000000000, -1.000000000000000000, 0.000000000000000000 ) ) ;
#8827 = DIRECTION ( 'NONE',  ( -1.000000000000000000, 0.000000000000000000, 0.000000000000000000 ) ) ;
#8828 = ORIENTED_EDGE ( 'NONE', *, *, #10657, .F. ) ;
#8829 = DIRECTION ( 'NONE',  ( 0.000000000000000000, 0.000000000000000000, -1.000000000000000000 ) ) ;
#8830 = CARTESIAN_POINT ( 'NONE',  ( 32.14641817400218571, 18.83615802559782182, -2.999999999999992450 ) ) ;
#8831 = EDGE_LOOP ( 'NONE', ( #10521, #14695, #21511, #2394, #11818, #22479 ) ) ;
#8832 = DIRECTION ( 'NONE',  ( 1.296372316667914327E-16, 1.000000000000000000, -0.000000000000000000 ) ) ;
#8833 = CARTESIAN_POINT ( 'NONE',  ( 19.51193873661505762, 31.10741194645160235, -57.96703944061300007 ) ) ;
#8834 = LINE ( 'NONE', #7229, #3508 ) ;
#8835 = DIRECTION ( 'NONE',  ( -0.000000000000000000, -0.000000000000000000, -1.000000000000000000 ) ) ;
#8836 = ORIENTED_EDGE ( 'NONE', *, *, #7501, .F. ) ;
#8837 = CARTESIAN_POINT ( 'NONE',  ( 12.99999999999993960, 42.51666049839543149, 100.0000000000000000 ) ) ;
#8838 = CARTESIAN_POINT ( 'NONE',  ( -2.175253701329903144, 39.97152389588116961, -50.35029005139294611 ) ) ;
#8839 = EDGE_CURVE ( 'NONE', #767, #13978, #1311, .T. ) ;
#8840 = ORIENTED_EDGE ( 'NONE', *, *, #19356, .T. ) ;
#8841 = CARTESIAN_POINT ( 'NONE',  ( 10.31465995609116604, 2.846668092511916992, 57.27881138849571840 ) ) ;
#8842 = AXIS2_PLACEMENT_3D ( 'NONE', #17107, #17446, #1424 ) ;
#8843 =( BOUNDED_SURFACE ( )  B_SPLINE_SURFACE ( 3, 2, ( 
 ( #16264, #21315, #15913 ),
 ( #7680, #9168, #9284 ),
 ( #5611, #2414, #5851 ),
 ( #14421, #21429, #7224 ),
 ( #697, #231, #4034 ),
 ( #7449, #9061, #14654 ) ),
 .UNSPECIFIED., .F., .F., .T. ) 
 B_SPLINE_SURFACE_WITH_KNOTS ( ( 4, 2, 4 ),
 ( 3, 3 ),
 ( -8.673617379884035472E-19, 0.002858401832365830338, 0.005716803664731661544 ),
 ( 0.000000000000000000, 1.000000000000000000 ),
 .UNSPECIFIED. ) 
 GEOMETRIC_REPRESENTATION_ITEM ( )  RATIONAL_B_SPLINE_SURFACE ( (
 ( 1.000000000000000000, 0.6290213284793358950, 1.000000000000000000),
 ( 1.000000000000000000, 0.6455195629496804921, 1.000000000000000000),
 ( 1.000000000000000000, 0.6615687397065170838, 1.000000000000000000),
 ( 1.000000000000000000, 0.6920701670982940534, 1.000000000000000000),
 ( 1.000000000000000000, 0.7065285139749719612, 1.000000000000000000),
 ( 1.000000000000000000, 0.7200096751079134716, 1.000000000000000000) ) ) 
 REPRESENTATION_ITEM ( '' )  SURFACE ( )  );
#8844 = CARTESIAN_POINT ( 'NONE',  ( 28.52469787935786982, 10.00000000000000000, -4.095854054471906203 ) ) ;
#8845 = DIRECTION ( 'NONE',  ( -0.000000000000000000, 1.000000000000000000, -0.000000000000000000 ) ) ;
#8846 = EDGE_CURVE ( 'NONE', #295, #20003, #15377, .T. ) ;
#8847 = VERTEX_POINT ( 'NONE', #1432 ) ;
#8848 = VERTEX_POINT ( 'NONE', #6934 ) ;
#8849 = VERTEX_POINT ( 'NONE', #10573 ) ;
#8850 = SHAPE_REPRESENTATION_RELATIONSHIP ( 'NONE' , 'NONE' ,  #3430, #14250 ) ;
#8851 = B_SPLINE_CURVE_WITH_KNOTS ( 'NONE', 3,
 ( #17287, #8253, #4719, #13269 ),
 .UNSPECIFIED., .F., .F.,
 ( 4, 4 ),
 ( 9.545285769181932779E-07, 0.001900595205834454448 ),
 .UNSPECIFIED. ) ;
#8852 = ORIENTED_EDGE ( 'NONE', *, *, #8209, .T. ) ;
#8853 = DIRECTION ( 'NONE',  ( 0.7071067811865524577, 8.659560562354993255E-17, -0.7071067811865426878 ) ) ;
#8854 = CARTESIAN_POINT ( 'NONE',  ( 13.56354382738800268, 2.142135623730931471, 56.03997097393685323 ) ) ;
#8855 = CARTESIAN_POINT ( 'NONE',  ( 9.689843208404393948, 39.33333333333333570, -54.54983754392740991 ) ) ;
#8856 = CARTESIAN_POINT ( 'NONE',  ( 2.026528946947714349, 40.00000000000001421, 49.98891164559377387 ) ) ;
#8857 = ADVANCED_FACE ( 'NONE', ( #4984 ), #7140, .T. ) ;
#8858 = EDGE_LOOP ( 'NONE', ( #12468, #14583, #7108, #5788 ) ) ;
#8859 = FACE_BOUND ( 'NONE', #3213, .T. ) ;
#8860 = FACE_OUTER_BOUND ( 'NONE', #18983, .T. ) ;
#8861 = ORIENTED_EDGE ( 'NONE', *, *, #9476, .T. ) ;
#8862 = CYLINDRICAL_SURFACE ( 'NONE', #589, 19.11328065563151313 ) ;
#8863 = DIRECTION ( 'NONE',  ( 6.505213034913038160E-19, 3.903127820947822896E-18, 1.000000000000000000 ) ) ;
#8864 = VERTEX_POINT ( 'NONE', #13990 ) ;
#8865 = CARTESIAN_POINT ( 'NONE',  ( 14.29266125237937857, -28.07080038625103668, -6.999999999999999112 ) ) ;
#8866 = ORIENTED_EDGE ( 'NONE', *, *, #14488, .F. ) ;
#8867 = CARTESIAN_POINT ( 'NONE',  ( 34.84717828836195253, -6.955395936296957515, -2.999999999999999556 ) ) ;
#8868 = EDGE_CURVE ( 'NONE', #21245, #22510, #8441, .T. ) ;
#8869 = FACE_OUTER_BOUND ( 'NONE', #16894, .T. ) ;
#8870 = CARTESIAN_POINT ( 'NONE',  ( -1.105958002183684119, 39.99272032066614457, 49.57516047002052773 ) ) ;
#8871 = CARTESIAN_POINT ( 'NONE',  ( 15.89815672374940725, 32.14246426897741316, 59.47617874060763654 ) ) ;
#8872 = CARTESIAN_POINT ( 'NONE',  ( 5.833333333333336590, 40.00000000000000000, 40.61164310337068173 ) ) ;
#8873 = DIRECTION ( 'NONE',  ( -1.000000000000000000, -7.260808888779397243E-16, 0.000000000000000000 ) ) ;
#8874 = CIRCLE ( 'NONE', #13980, 19.11328065563152379 ) ;
#8875 = ORIENTED_EDGE ( 'NONE', *, *, #7534, .F. ) ;
#8876 = ORIENTED_EDGE ( 'NONE', *, *, #16352, .F. ) ;
#8877 = ORIENTED_EDGE ( 'NONE', *, *, #15916, .F. ) ;
#8878 = ORIENTED_EDGE ( 'NONE', *, *, #13645, .T. ) ;
#8879 = CARTESIAN_POINT ( 'NONE',  ( -12.27586057105639661, 4.193657236093902618, 55.54740530680980015 ) ) ;
#8880 = CARTESIAN_POINT ( 'NONE',  ( 35.00000000000001421, -5.000000000000000000, 59.99999999999703704 ) ) ;
#8881 = ADVANCED_FACE ( 'NONE', ( #10456 ), #12781, .F. ) ;
#8882 = B_SPLINE_CURVE_WITH_KNOTS ( 'NONE', 3,
 ( #18727, #16785, #20114, #1090, #853, #3034, #1190, #8083, #973, #22057, #6350, #14705, #7844 ),
 .UNSPECIFIED., .F., .F.,
 ( 4, 2, 1, 1, 1, 2, 2, 4 ),
 ( 0.000000000000000000, 0.2499999999999845124, 0.3749999999999741318, 0.4374999999999714673, 0.4687499999999691358, 0.4843749999999679146, 0.4999999999999667488, 1.000000000000000000 ),
 .UNSPECIFIED. ) ;
#8883 = LINE ( 'NONE', #15754, #19348 ) ;
#8884 = CARTESIAN_POINT ( 'NONE',  ( 4.573707224651647252, 39.86977587139770662, 51.94771479820464322 ) ) ;
#8885 = AXIS2_PLACEMENT_3D ( 'NONE', #21552, #21895, #913 ) ;
#8886 = AXIS2_PLACEMENT_3D ( 'NONE', #19094, #8995, #10591 ) ;
#8887 = VERTEX_POINT ( 'NONE', #16415 ) ;
#8888 = CARTESIAN_POINT ( 'NONE',  ( 23.49999999999998579, 19.99999999999999645, 105.0000000000000142 ) ) ;
#8889 = LINE ( 'NONE', #10707, #970 ) ;
#8890 = EDGE_CURVE ( 'NONE', #11380, #19753, #16853, .T. ) ;
#8891 = DIRECTION ( 'NONE',  ( -1.296372316667914327E-16, -1.000000000000000000, 0.000000000000000000 ) ) ;
#8892 = EDGE_CURVE ( 'NONE', #3556, #6991, #1986, .T. ) ;
#8893 = CARTESIAN_POINT ( 'NONE',  ( -34.11307262910428761, 11.98990878915333091, -2.932164912090547748 ) ) ;
#8894 = VECTOR ( 'NONE', #12519, 1000.000000000000000 ) ;
#8895 = LINE ( 'NONE', #5244, #21731 ) ;
#8896 = DIRECTION ( 'NONE',  ( 1.000000000000000000, 0.000000000000000000, 0.000000000000000000 ) ) ;
#8897 = CARTESIAN_POINT ( 'NONE',  ( -24.43568323314231350, 26.65040777864162536, 2.932460736555809966 ) ) ;
#8898 = EDGE_CURVE ( 'NONE', #22152, #18617, #16729, .T. ) ;
#8899 = ORIENTED_EDGE ( 'NONE', *, *, #11274, .T. ) ;
#8900 = CIRCLE ( 'NONE', #7791, 36.76383501243555685 ) ;
#8901 = ORIENTED_EDGE ( 'NONE', *, *, #11138, .T. ) ;
#8902 = CIRCLE ( 'NONE', #10720, 2.000000000000002665 ) ;
#8903 = CIRCLE ( 'NONE', #847, 2.099999999999997868 ) ;
#8904 = VERTEX_POINT ( 'NONE', #729 ) ;
#8905 = CARTESIAN_POINT ( 'NONE',  ( 10.27431133777639793, -4.928932188134518277, -51.43682631505696179 ) ) ;
#8906 = ADVANCED_FACE ( 'NONE', ( #14453 ), #7711, .T. ) ;
#8907 = CARTESIAN_POINT ( 'NONE',  ( 11.16030968682943225, 40.00000000000000711, -54.02479386262969996 ) ) ;
#8908 = CARTESIAN_POINT ( 'NONE',  ( 2.775557561562891351E-14, 2.775557561562891351E-14, 5.750000000000001776 ) ) ;
#8909 = CIRCLE ( 'NONE', #1606, 2.099999999999997868 ) ;
#8910 = CARTESIAN_POINT ( 'NONE',  ( 22.15900668633799597, 29.33526866242080899, -2.800654218530477912 ) ) ;
#8911 = DIRECTION ( 'NONE',  ( 1.000000000000000000, 1.208970125616053321E-17, 0.000000000000000000 ) ) ;
#8912 = PLANE ( 'NONE',  #14155 ) ;
#8913 = DIRECTION ( 'NONE',  ( -1.000000000000000000, 0.000000000000000000, 0.000000000000000000 ) ) ;
#8914 = CIRCLE ( 'NONE', #2339, 25.00000000000000711 ) ;
#8915 = ORIENTED_EDGE ( 'NONE', *, *, #15572, .T. ) ;
#8916 = CARTESIAN_POINT ( 'NONE',  ( 2.220446049250313081E-13, -2.498001805406602216E-13, -6.859353255829918616 ) ) ;
#8917 = FACE_BOUND ( 'NONE', #5338, .T. ) ;
#8918 = VECTOR ( 'NONE', #9500, 1000.000000000000000 ) ;
#8919 = LINE ( 'NONE', #1934, #3168 ) ;
#8920 = CARTESIAN_POINT ( 'NONE',  ( 13.76792553423403831, 13.99810558461767407, -45.26963775109937416 ) ) ;
#8921 = AXIS2_PLACEMENT_3D ( 'NONE', #22471, #3563, #10296 ) ;
#8922 = EDGE_CURVE ( 'NONE', #17550, #1088, #19543, .T. ) ;
#8923 = ORIENTED_EDGE ( 'NONE', *, *, #19973, .F. ) ;
#8924 = EDGE_CURVE ( 'NONE', #9113, #8307, #11140, .T. ) ;
#8925 = LINE ( 'NONE', #12361, #11184 ) ;
#8926 = DIRECTION ( 'NONE',  ( 0.000000000000000000, 0.000000000000000000, -1.000000000000000000 ) ) ;
#8927 = EDGE_CURVE ( 'NONE', #15891, #16318, #16537, .T. ) ;
#8928 = AXIS2_PLACEMENT_3D ( 'NONE', #2230, #21480, #18153 ) ;
#8929 = ORIENTED_EDGE ( 'NONE', *, *, #10441, .F. ) ;
#8930 = VECTOR ( 'NONE', #5365, 1000.000000000000000 ) ;
#8931 = AXIS2_PLACEMENT_3D ( 'NONE', #22123, #2651, #1038 ) ;
#8932 = ORIENTED_EDGE ( 'NONE', *, *, #9040, .F. ) ;
#8933 = CARTESIAN_POINT ( 'NONE',  ( -0.7857880201000499998, 25.00083595504925071, 9.000278651543347053 ) ) ;
#8934 = LINE ( 'NONE', #17536, #8060 ) ;
#8935 = DIRECTION ( 'NONE',  ( 1.000000000000000000, 0.000000000000000000, 0.000000000000000000 ) ) ;
#8936 = VERTEX_POINT ( 'NONE', #14224 ) ;
#8937 = DIRECTION ( 'NONE',  ( 1.296372316667914327E-16, 1.000000000000000000, -0.000000000000000000 ) ) ;
#8938 = CARTESIAN_POINT ( 'NONE',  ( -8.105728697730361532, 40.00000000000000000, 53.00649037880594250 ) ) ;
#8939 = ORIENTED_EDGE ( 'NONE', *, *, #14173, .T. ) ;
#8940 = DIRECTION ( 'NONE',  ( -0.000000000000000000, 1.000000000000000000, -0.000000000000000000 ) ) ;
#8941 = FACE_OUTER_BOUND ( 'NONE', #2491, .T. ) ;
#8942 = LINE ( 'NONE', #20884, #20687 ) ;
#8943 = DIRECTION ( 'NONE',  ( 0.000000000000000000, 0.000000000000000000, -1.000000000000000000 ) ) ;
#8944 = ORIENTED_EDGE ( 'NONE', *, *, #12017, .T. ) ;
#8945 = DIRECTION ( 'NONE',  ( 0.000000000000000000, -1.000000000000000000, 0.000000000000000000 ) ) ;
#8946 = AXIS2_PLACEMENT_3D ( 'NONE', #20595, #20491, #17263 ) ;
#8947 = CARTESIAN_POINT ( 'NONE',  ( -16.06969024216325792, -19.15111107797470780, -4.999999999999969802 ) ) ;
#8948 = CARTESIAN_POINT ( 'NONE',  ( -4.556497549088540211, 39.87079204719141501, -51.93698204320140377 ) ) ;
#8949 = AXIS2_PLACEMENT_3D ( 'NONE', #21646, #7432, #16128 ) ;
#8950 = ORIENTED_EDGE ( 'NONE', *, *, #4299, .T. ) ;
#8951 = CARTESIAN_POINT ( 'NONE',  ( -8.550503583141495056, 23.49231551964756193, 3.000000000000023537 ) ) ;
#8952 = CARTESIAN_POINT ( 'NONE',  ( -7.505578006075205089, 1.461761173328240515, 55.63523492904089096 ) ) ;
#8953 = AXIS2_PLACEMENT_3D ( 'NONE', #5118, #16928, #9936 ) ;
#8954 = ORIENTED_EDGE ( 'NONE', *, *, #16549, .T. ) ;
#8955 = ORIENTED_EDGE ( 'NONE', *, *, #4401, .T. ) ;
#8956 = AXIS2_PLACEMENT_3D ( 'NONE', #18291, #9579, #18640 ) ;
#8957 = EDGE_LOOP ( 'NONE', ( #16141, #3902 ) ) ;
#8958 = EDGE_CURVE ( 'NONE', #4779, #1795, #5531, .T. ) ;
#8959 = VERTEX_POINT ( 'NONE', #10913 ) ;
#8960 = CYLINDRICAL_SURFACE ( 'NONE', #18357, 0.9999999999999974465 ) ;
#8961 = CIRCLE ( 'NONE', #15165, 2.099999999999997868 ) ;
#8962 = CYLINDRICAL_SURFACE ( 'NONE', #15994, 20.00000000000000000 ) ;
#8963 = CARTESIAN_POINT ( 'NONE',  ( 3.022692775171828217, 39.94544418562367838, -50.94009349721213198 ) ) ;
#8964 = CARTESIAN_POINT ( 'NONE',  ( 8.578904124028513323, 40.00000000000000000, 53.18551242646393717 ) ) ;
#8965 = VERTEX_POINT ( 'NONE', #11028 ) ;
#8966 = DIRECTION ( 'NONE',  ( -1.000000000000000000, 0.000000000000000000, 0.000000000000000000 ) ) ;
#8967 = DIRECTION ( 'NONE',  ( 0.000000000000000000, 0.000000000000000000, -1.000000000000000000 ) ) ;
#8968 = ORIENTED_EDGE ( 'NONE', *, *, #5114, .T. ) ;
#8969 = CARTESIAN_POINT ( 'NONE',  ( -1.436159831096171624, -1.268900497114691772, 49.23900052097178559 ) ) ;
#8970 = LINE ( 'NONE', #2100, #7902 ) ;
#8971 = EDGE_CURVE ( 'NONE', #7032, #4351, #3827, .T. ) ;
#8972 = CARTESIAN_POINT ( 'NONE',  ( 17.99999999999998579, 20.00000000000000355, 105.0000000000000142 ) ) ;
#8973 = VERTEX_POINT ( 'NONE', #10790 ) ;
#8974 = DIRECTION ( 'NONE',  ( -0.000000000000000000, -0.000000000000000000, 1.000000000000000000 ) ) ;
#8975 = EDGE_LOOP ( 'NONE', ( #237, #15390, #14809, #19481 ) ) ;
#8976 = CYLINDRICAL_SURFACE ( 'NONE', #2797, 8.999999999999998224 ) ;
#8977 = AXIS2_PLACEMENT_3D ( 'NONE', #10769, #19170, #14086 ) ;
#8978 = DIRECTION ( 'NONE',  ( 1.296372316667914327E-16, 1.000000000000000000, -0.000000000000000000 ) ) ;
#8979 = CARTESIAN_POINT ( 'NONE',  ( 25.00000000000000000, 20.00000000000000000, 6.487780019669002523E-15 ) ) ;
#8980 = VECTOR ( 'NONE', #3554, 1000.000000000000114 ) ;
#8981 = CARTESIAN_POINT ( 'NONE',  ( 8.732266002733743093, 39.99999999999999289, -53.24192878695249931 ) ) ;
#8982 = CARTESIAN_POINT ( 'NONE',  ( 19.97049456717391891, 21.17381189076418124, 60.61481192459388723 ) ) ;
#8983 = DIRECTION ( 'NONE',  ( 0.000000000000000000, -0.000000000000000000, -1.000000000000000000 ) ) ;
#8984 = AXIS2_PLACEMENT_3D ( 'NONE', #3469, #22382, #13629 ) ;
#8985 = AXIS2_PLACEMENT_3D ( 'NONE', #3861, #17604, #8791 ) ;
#8986 = CARTESIAN_POINT ( 'NONE',  ( 35.00000000000000000, -4.928932188134504955, 57.07106781186552524 ) ) ;
#8987 = VERTEX_POINT ( 'NONE', #2099 ) ;
#8988 = VERTEX_POINT ( 'NONE', #17912 ) ;
#8989 = ORIENTED_EDGE ( 'NONE', *, *, #3031, .F. ) ;
#8990 = CONICAL_SURFACE ( 'NONE', #21084, 3.399999999999995026, 1.029744258676652313 ) ;
#8991 = EDGE_CURVE ( 'NONE', #9647, #2304, #17079, .T. ) ;
#8992 = TOROIDAL_SURFACE ( 'NONE', #15568, 34.90673715956759082, 8.750000000000000000 ) ;
#8993 = ORIENTED_EDGE ( 'NONE', *, *, #1183, .T. ) ;
#8994 = CARTESIAN_POINT ( 'NONE',  ( 4.170748987303491084, -34.65667543218836499, -2.999999999999988898 ) ) ;
#8995 = DIRECTION ( 'NONE',  ( -0.000000000000000000, 1.000000000000000000, -0.000000000000000000 ) ) ;
#8996 = CARTESIAN_POINT ( 'NONE',  ( 34.99999999999999289, 0.000000000000000000, -54.99999999999705835 ) ) ;
#8997 = B_SPLINE_CURVE_WITH_KNOTS ( 'NONE', 3,
 ( #10422, #13622, #10310, #10537, #15700, #1739, #8723, #15, #20984, #10203, #5073, #8492 ),
 .UNSPECIFIED., .F., .F.,
 ( 4, 1, 1, 1, 1, 2, 2, 4 ),
 ( 0.000000000000000000, 0.2500000000000013323, 0.3750000000000022760, 0.4375000000000013878, 0.4687500000000019984, 0.4843750000000033862, 0.5000000000000047740, 1.000000000000000000 ),
 .UNSPECIFIED. ) ;
#8998 = FACE_OUTER_BOUND ( 'NONE', #11134, .T. ) ;
#8999 = DIRECTION ( 'NONE',  ( -0.000000000000000000, 1.000000000000000000, -0.000000000000000000 ) ) ;
#9000 = CARTESIAN_POINT ( 'NONE',  ( 0.03025501645077945459, 39.99999465686278199, 48.75751133701592011 ) ) ;
#9001 = EDGE_CURVE ( 'NONE', #20362, #4023, #19863, .T. ) ;
#9002 = ORIENTED_EDGE ( 'NONE', *, *, #6708, .T. ) ;
#9003 = DIRECTION ( 'NONE',  ( 0.000000000000000000, -1.000000000000000000, 0.000000000000000000 ) ) ;
#9004 = DIRECTION ( 'NONE',  ( -6.505213034913038160E-19, -3.903127820947822896E-18, -1.000000000000000000 ) ) ;
#9005 = DIRECTION ( 'NONE',  ( 1.296372316667914327E-16, 1.000000000000000000, -0.000000000000000000 ) ) ;
#9006 = LINE ( 'NONE', #14259, #15918 ) ;
#9007 = CYLINDRICAL_SURFACE ( 'NONE', #13481, 2.500000000000002220 ) ;
#9008 = CARTESIAN_POINT ( 'NONE',  ( -18.87121696173700514, 26.69448804128720099, 60.34297443853448328 ) ) ;
#9009 = CIRCLE ( 'NONE', #17794, 8.999999999999966249 ) ;
#9010 = AXIS2_PLACEMENT_3D ( 'NONE', #4448, #16578, #885 ) ;
#9011 = AXIS2_PLACEMENT_3D ( 'NONE', #13415, #20546, #13296 ) ;
#9012 = CONICAL_SURFACE ( 'NONE', #21841, 18.00000000000000000, 0.7853981633974540522 ) ;
#9013 = FACE_OUTER_BOUND ( 'NONE', #10497, .T. ) ;
#9014 = EDGE_CURVE ( 'NONE', #21600, #16362, #14525, .T. ) ;
#9015 = CYLINDRICAL_SURFACE ( 'NONE', #21111, 20.00000000000000000 ) ;
#9016 = ORIENTED_EDGE ( 'NONE', *, *, #11783, .F. ) ;
#9017 = AXIS2_PLACEMENT_3D ( 'NONE', #13824, #22443, #20841 ) ;
#9018 = ORIENTED_EDGE ( 'NONE', *, *, #15267, .F. ) ;
#9019 = ADVANCED_FACE ( 'NONE', ( #7596 ), #6492, .T. ) ;
#9020 = ORIENTED_EDGE ( 'NONE', *, *, #7122, .F. ) ;
#9021 = CARTESIAN_POINT ( 'NONE',  ( 3.001573872050378622, -1.099462678408570149, -50.31569927527887387 ) ) ;
#9022 = CARTESIAN_POINT ( 'NONE',  ( -32.89319786336240270, -15.00354810072223977, -2.933296326616348093 ) ) ;
#9023 = AXIS2_PLACEMENT_3D ( 'NONE', #2045, #22584, #10398 ) ;
#9024 = DIRECTION ( 'NONE',  ( 6.505213034913038160E-19, 3.903127820947822896E-18, 1.000000000000000000 ) ) ;
#9025 = CARTESIAN_POINT ( 'NONE',  ( 0.000000000000000000, 9.999999999999998224, 0.000000000000000000 ) ) ;
#9026 = EDGE_CURVE ( 'NONE', #8041, #16345, #16366, .T. ) ;
#9027 = DIRECTION ( 'NONE',  ( 0.000000000000000000, 0.000000000000000000, 1.000000000000000000 ) ) ;
#9028 = CARTESIAN_POINT ( 'NONE',  ( -17.38307674301858796, 10.07685590252459029, 59.93367040492846343 ) ) ;
#9029 = CARTESIAN_POINT ( 'NONE',  ( -13.25803659942197754, 34.99815359651601909, -58.54720450724500580 ) ) ;
#9030 = CARTESIAN_POINT ( 'NONE',  ( 5.673811190418850800E-15, 6.776263578034402713E-17, -18.00000000000000711 ) ) ;
#9031 = AXIS2_PLACEMENT_3D ( 'NONE', #5296, #14515, #14395 ) ;
#9032 = VERTEX_POINT ( 'NONE', #7820 ) ;
#9033 = CARTESIAN_POINT ( 'NONE',  ( -18.22261011550280330, -31.92986134326242365, -2.000000000000005329 ) ) ;
#9034 = CARTESIAN_POINT ( 'NONE',  ( -19.99999999999998579, 28.19616000222404040, 0.000000000000000000 ) ) ;
#9035 =( NAMED_UNIT ( * ) PLANE_ANGLE_UNIT ( ) SI_UNIT ( $, .RADIAN. ) );
#9036 = EDGE_CURVE ( 'NONE', #22537, #13925, #13790, .T. ) ;
#9037 = DIRECTION ( 'NONE',  ( 6.505213034913038160E-19, 3.903127820947822896E-18, 1.000000000000000000 ) ) ;
#9038 = DIRECTION ( 'NONE',  ( 0.000000000000000000, 0.000000000000000000, 1.000000000000000000 ) ) ;
#9039 = ORIENTED_EDGE ( 'NONE', *, *, #1610, .T. ) ;
#9040 = EDGE_CURVE ( 'NONE', #17179, #8864, #14452, .T. ) ;
#9041 = CARTESIAN_POINT ( 'NONE',  ( 42.50000000000000711, -9.600000000000001421, 45.40000000000001279 ) ) ;
#9042 = AXIS2_PLACEMENT_3D ( 'NONE', #16972, #6222, #1068 ) ;
#9043 = DIRECTION ( 'NONE',  ( -1.000000000000000000, 0.000000000000000000, 0.000000000000000000 ) ) ;
#9044 = AXIS2_PLACEMENT_3D ( 'NONE', #16603, #7556, #20052 ) ;
#9045 = DIRECTION ( 'NONE',  ( -0.000000000000000000, -1.000000000000000000, -0.000000000000000000 ) ) ;
#9046 = EDGE_CURVE ( 'NONE', #3399, #19609, #640, .T. ) ;
#9047 = VERTEX_POINT ( 'NONE', #11485 ) ;
#9048 = AXIS2_PLACEMENT_3D ( 'NONE', #12261, #11, #19152 ) ;
#9049 = ITEM_DEFINED_TRANSFORMATION ( 'NONE', 'NONE', #19003,  #18273 ) ;
#9050 = EDGE_CURVE ( 'NONE', #12342, #3379, #7205, .T. ) ;
#9051 = ORIENTED_EDGE ( 'NONE', *, *, #18428, .T. ) ;
#9052 = CARTESIAN_POINT ( 'NONE',  ( 0.2369875743634299314, 39.99966999001385659, -48.91756785322892398 ) ) ;
#9053 = CIRCLE ( 'NONE', #2855, 1.000000000000000888 ) ;
#9054 = CARTESIAN_POINT ( 'NONE',  ( -10.60627602730582275, 0.5940385038083396685, 54.69850067894232382 ) ) ;
#9055 = CARTESIAN_POINT ( 'NONE',  ( -34.99999999999981526, 24.73819270004212356, 54.99999999999922551 ) ) ;
#9056 = FACE_OUTER_BOUND ( 'NONE', #18481, .T. ) ;
#9057 = VECTOR ( 'NONE', #16923, 1000.000000000000000 ) ;
#9058 = EDGE_CURVE ( 'NONE', #22614, #21019, #13424, .T. ) ;
#9059 = ORIENTED_EDGE ( 'NONE', *, *, #20824, .F. ) ;
#9060 = LINE ( 'NONE', #16036, #1579 ) ;
#9061 = CARTESIAN_POINT ( 'NONE',  ( -8.349099696861340902, 1.803277857259562245, -53.93591755799871379 ) ) ;
#9062 = VERTEX_POINT ( 'NONE', #11255 ) ;
#9063 = DIRECTION ( 'NONE',  ( 0.000000000000000000, -1.000000000000000000, 0.000000000000000000 ) ) ;
#9064 = VECTOR ( 'NONE', #22424, 999.9999999999998863 ) ;
#9065 = CARTESIAN_POINT ( 'NONE',  ( 14.95260096911750303, 3.243207204902308405, -56.55590526898570403 ) ) ;
#9066 = CARTESIAN_POINT ( 'NONE',  ( 42.50000000000000711, -12.00000000000000000, 47.50000000000000711 ) ) ;
#9067 = EDGE_CURVE ( 'NONE', #17893, #15849, #18253, .T. ) ;
#9068 = VERTEX_POINT ( 'NONE', #13286 ) ;
#9069 = DIRECTION ( 'NONE',  ( 6.505213034913038160E-19, 3.903127820947822896E-18, 1.000000000000000000 ) ) ;
#9070 = DIRECTION ( 'NONE',  ( 0.000000000000000000, -1.000000000000000000, 0.000000000000000000 ) ) ;
#9071 = CARTESIAN_POINT ( 'NONE',  ( -0.5323815408128229620, 39.99832331801214735, -49.14386499772781036 ) ) ;
#9072 = ORIENTED_EDGE ( 'NONE', *, *, #15246, .F. ) ;
#9073 = CIRCLE ( 'NONE', #4336, 30.00000000000000000 ) ;
#9074 = CARTESIAN_POINT ( 'NONE',  ( 90.00000000000000000, 39.97500000000000142, 2.500000000000001332 ) ) ;
#9075 = CARTESIAN_POINT ( 'NONE',  ( 27.19760187735878532, 24.73600648735102681, -2.800654218530485018 ) ) ;
#9076 = AXIS2_PLACEMENT_3D ( 'NONE', #15093, #4367, #15212 ) ;
#9077 = VECTOR ( 'NONE', #6257, 1000.000000000000000 ) ;
#9078 = AXIS2_PLACEMENT_3D ( 'NONE', #1060, #6217, #21687 ) ;
#9079 = ORIENTED_EDGE ( 'NONE', *, *, #3000, .F. ) ;
#9080 = VERTEX_POINT ( 'NONE', #2564 ) ;
#9081 = ORIENTED_EDGE ( 'NONE', *, *, #5601, .F. ) ;
#9082 = EDGE_CURVE ( 'NONE', #1418, #11275, #11600, .T. ) ;
#9083 = ORIENTED_EDGE ( 'NONE', *, *, #848, .T. ) ;
#9084 = DIRECTION ( 'NONE',  ( 0.000000000000000000, 1.000000000000000000, 0.000000000000000000 ) ) ;
#9085 = DIRECTION ( 'NONE',  ( -1.000000000000000000, 0.000000000000000000, 0.000000000000000000 ) ) ;
#9086 = FACE_OUTER_BOUND ( 'NONE', #13675, .T. ) ;
#9087 = FACE_OUTER_BOUND ( 'NONE', #657, .T. ) ;
#9088 = AXIS2_PLACEMENT_3D ( 'NONE', #9962, #6648, #3220 ) ;
#9089 = ORIENTED_EDGE ( 'NONE', *, *, #8924, .T. ) ;
#9090 = CARTESIAN_POINT ( 'NONE',  ( 35.00000000000000711, -5.000000000000000000, -57.00000000000001421 ) ) ;
#9091 = CARTESIAN_POINT ( 'NONE',  ( -28.96193690644914653, -14.74639653023232455, -6.999999999999950262 ) ) ;
#9092 = ORIENTED_EDGE ( 'NONE', *, *, #3448, .T. ) ;
#9093 = DIRECTION ( 'NONE',  ( 0.000000000000000000, 0.000000000000000000, -1.000000000000000000 ) ) ;
#9094 = CARTESIAN_POINT ( 'NONE',  ( -12.60179598819648739, 38.53795549125497644, -55.66391160832503004 ) ) ;
#9095 = CIRCLE ( 'NONE', #21910, 11.99999999999985434 ) ;
#9096 = AXIS2_PLACEMENT_3D ( 'NONE', #7487, #5771, #16534 ) ;
#9097 = CARTESIAN_POINT ( 'NONE',  ( 0.000000000000000000, 30.00000000000000355, 0.000000000000000000 ) ) ;
#9098 = ORIENTED_EDGE ( 'NONE', *, *, #16254, .F. ) ;
#9099 = CARTESIAN_POINT ( 'NONE',  ( 2.220446049250313081E-13, -8.326672684688674053E-14, 2.800654218530498785 ) ) ;
#9100 = EDGE_CURVE ( 'NONE', #691, #1737, #19314, .T. ) ;
#9101 = ORIENTED_EDGE ( 'NONE', *, *, #12803, .F. ) ;
#9102 = CARTESIAN_POINT ( 'NONE',  ( -3.286600300096431288E-14, 40.00000000000000000, -48.73397172404478539 ) ) ;
#9103 = CARTESIAN_POINT ( 'NONE',  ( -2.546709079545449672, 39.84786395731773467, 51.61893211308341023 ) ) ;
#9104 = SURFACE_SIDE_STYLE ('',( #10679 ) ) ;
#9105 = ORIENTED_EDGE ( 'NONE', *, *, #20235, .T. ) ;
#9106 = CARTESIAN_POINT ( 'NONE',  ( 21.60080777693143972, 26.06115151610029912, 58.48488838346896301 ) ) ;
#9107 = CARTESIAN_POINT ( 'NONE',  ( -42.50000000000000000, 7.000000000000000000, 49.99999999999999289 ) ) ;
#9108 = CARTESIAN_POINT ( 'NONE',  ( 11.88509939555964046, 36.18356491089507188, -55.39957109942752567 ) ) ;
#9109 = CONICAL_SURFACE ( 'NONE', #15302, 2.524999999999999467, 0.7853981633974482790 ) ;
#9110 = CONICAL_SURFACE ( 'NONE', #8372, 19.99999999999999289, 1.308996938995746984 ) ;
#9111 = ORIENTED_EDGE ( 'NONE', *, *, #20140, .T. ) ;
#9112 = EDGE_CURVE ( 'NONE', #18984, #12705, #11710, .T. ) ;
#9113 = VERTEX_POINT ( 'NONE', #1169 ) ;
#9114 = VERTEX_POINT ( 'NONE', #22147 ) ;
#9115 = PRODUCT_DEFINITION_FORMATION_WITH_SPECIFIED_SOURCE ( 'ANY', '', #2548, .NOT_KNOWN. ) ;
#9116 = ORIENTED_EDGE ( 'NONE', *, *, #7713, .F. ) ;
#9117 = FACE_OUTER_BOUND ( 'NONE', #14616, .T. ) ;
#9118 = CARTESIAN_POINT ( 'NONE',  ( -10.84015308335310479, 39.16451817969218041, -54.95776488303458507 ) ) ;
#9119 = DIRECTION ( 'NONE',  ( 0.000000000000000000, 0.7071067811865326957, 0.7071067811865622277 ) ) ;
#9120 = DIRECTION ( 'NONE',  ( 0.000000000000000000, 0.000000000000000000, 1.000000000000000000 ) ) ;
#9121 = CARTESIAN_POINT ( 'NONE',  ( 42.50000000000000711, -12.00000000000000000, -45.00000000000000000 ) ) ;
#9122 = AXIS2_PLACEMENT_3D ( 'NONE', #21386, #4091, #7637 ) ;
#9123 = ORIENTED_EDGE ( 'NONE', *, *, #18406, .T. ) ;
#9124 = FACE_OUTER_BOUND ( 'NONE', #12730, .T. ) ;
#9125 = LINE ( 'NONE', #1808, #14169 ) ;
#9126 = DIRECTION ( 'NONE',  ( 0.000000000000000000, 0.000000000000000000, 1.000000000000000000 ) ) ;
#9127 = DIRECTION ( 'NONE',  ( 0.000000000000000000, 0.000000000000000000, 1.000000000000000000 ) ) ;
#9128 = DIRECTION ( 'NONE',  ( 0.000000000000000000, 0.000000000000000000, -1.000000000000000000 ) ) ;
#9129 = EDGE_CURVE ( 'NONE', #10746, #9068, #3353, .T. ) ;
#9130 = PRODUCT_RELATED_PRODUCT_CATEGORY ( 'part', '', ( #20116 ) ) ;
#9131 = FACE_BOUND ( 'NONE', #10075, .T. ) ;
#9132 = LINE ( 'NONE', #19681, #5729 ) ;
#9133 = ORIENTED_EDGE ( 'NONE', *, *, #15477, .T. ) ;
#9134 = EDGE_CURVE ( 'NONE', #5841, #11067, #17464, .T. ) ;
#9135 = ORIENTED_EDGE ( 'NONE', *, *, #8846, .T. ) ;
#9136 = VECTOR ( 'NONE', #21473, 1000.000000000000000 ) ;
#9137 = B_SPLINE_CURVE_WITH_KNOTS ( 'NONE', 3,
 ( #15226, #22246, #15342, #11910, #22361, #6124 ),
 .UNSPECIFIED., .F., .F.,
 ( 4, 2, 4 ),
 ( 3.576224061345498009E-18, 0.003173601132114241274, 0.006347202264228479079 ),
 .UNSPECIFIED. ) ;
#9138 = ORIENTED_EDGE ( 'NONE', *, *, #19693, .F. ) ;
#9139 = FACE_OUTER_BOUND ( 'NONE', #22418, .T. ) ;
#9140 = CARTESIAN_POINT ( 'NONE',  ( 11.59091061707581893, 40.00000000000000000, -54.17810196248734655 ) ) ;
#9141 = CARTESIAN_POINT ( 'NONE',  ( 44.60000000000000853, -9.600000000000001421, 47.50000000000000711 ) ) ;
#9142 = CARTESIAN_POINT ( 'NONE',  ( 20.55056392469605342, -29.75120097320042944, -2.932164912090510889 ) ) ;
#9143 = EDGE_CURVE ( 'NONE', #19192, #11430, #10499, .T. ) ;
#9144 = DIRECTION ( 'NONE',  ( -0.000000000000000000, 1.000000000000000000, -0.000000000000000000 ) ) ;
#9145 = LINE ( 'NONE', #16116, #4702 ) ;
#9146 = DIRECTION ( 'NONE',  ( -1.445602896647339163E-16, 0.000000000000000000, -1.000000000000000000 ) ) ;
#9147 = CARTESIAN_POINT ( 'NONE',  ( -10.35112103033871556, 34.64554704988846368, -2.932164912090562847 ) ) ;
#9148 = CIRCLE ( 'NONE', #19766, 36.76383501243555685 ) ;
#9149 = ORIENTED_EDGE ( 'NONE', *, *, #4829, .F. ) ;
#9150 = LINE ( 'NONE', #19703, #6861 ) ;
#9151 = DIRECTION ( 'NONE',  ( -1.000000000000000000, 0.000000000000000000, 0.000000000000000000 ) ) ;
#9152 = DIRECTION ( 'NONE',  ( 0.000000000000000000, 0.000000000000000000, -1.000000000000000000 ) ) ;
#9153 = EDGE_CURVE ( 'NONE', #21800, #22583, #20643, .T. ) ;
#9154 = CARTESIAN_POINT ( 'NONE',  ( 4.170748987303435129, -34.65667543218869895, 2.999999999999999112 ) ) ;
#9155 = ORIENTED_EDGE ( 'NONE', *, *, #22665, .T. ) ;
#9156 = CARTESIAN_POINT ( 'NONE',  ( -21.00948735876882623, -24.79619811426206510, -6.999999999999950262 ) ) ;
#9157 = DIRECTION ( 'NONE',  ( 0.000000000000000000, -0.000000000000000000, 1.000000000000000000 ) ) ;
#9158 = AXIS2_PLACEMENT_3D ( 'NONE', #20566, #980, #21961 ) ;
#9159 = ORIENTED_EDGE ( 'NONE', *, *, #12120, .T. ) ;
#9160 = CONTEXT_DEPENDENT_SHAPE_REPRESENTATION ( #21306, #21752 ) ;
#9161 = ORIENTED_EDGE ( 'NONE', *, *, #9153, .T. ) ;
#9162 = CARTESIAN_POINT ( 'NONE',  ( -2.999999999999999556, 22.00000000000000355, 6.485281374238567764 ) ) ;
#9163 = CARTESIAN_POINT ( 'NONE',  ( 26.79308242454903066, 16.56444186175090749, -2.999999999999971578 ) ) ;
#9164 = EDGE_CURVE ( 'NONE', #11367, #31, #17184, .T. ) ;
#9165 = CARTESIAN_POINT ( 'NONE',  ( 11.98990878915362757, 34.11307262910417393, -2.932164912090556186 ) ) ;
#9166 = VERTEX_POINT ( 'NONE', #15584 ) ;
#9167 = DIRECTION ( 'NONE',  ( -6.505213034913038160E-19, -3.903127820947822896E-18, -1.000000000000000000 ) ) ;
#9168 = CARTESIAN_POINT ( 'NONE',  ( -11.68987541777273265, 3.735186999524350959, -55.40064774186661367 ) ) ;
#9169 = ORIENTED_EDGE ( 'NONE', *, *, #9545, .F. ) ;
#9170 = DIRECTION ( 'NONE',  ( 0.000000000000000000, 0.000000000000000000, 1.000000000000000000 ) ) ;
#9171 = CARTESIAN_POINT ( 'NONE',  ( -27.56232195404058416, 21.41958700883256483, -2.999999999999971578 ) ) ;
#9172 = LINE ( 'NONE', #14547, #10803 ) ;
#9173 = AXIS2_PLACEMENT_3D ( 'NONE', #11840, #20673, #15384 ) ;
#9174 = LINE ( 'NONE', #7455, #18453 ) ;
#9175 = ORIENTED_EDGE ( 'NONE', *, *, #6074, .F. ) ;
#9176 = CARTESIAN_POINT ( 'NONE',  ( 1.128083539116558898, 34.88850421923955736, 3.000000000000002665 ) ) ;
#9177 = CYLINDRICAL_SURFACE ( 'NONE', #1612, 36.76383501243555685 ) ;
#9178 = ADVANCED_FACE ( 'NONE', ( #1397 ), #3579, .F. ) ;
#9179 = EDGE_CURVE ( 'NONE', #21079, #11081, #12051, .T. ) ;
#9180 = CARTESIAN_POINT ( 'NONE',  ( -41.39271818392631985, 10.00000000000000000, 5.943569790512528428 ) ) ;
#9181 = EDGE_CURVE ( 'NONE', #18812, #21534, #22223, .T. ) ;
#9182 = EDGE_LOOP ( 'NONE', ( #10531, #5419, #20690 ) ) ;
#9183 = CARTESIAN_POINT ( 'NONE',  ( -36.39375341857525825, -7.980461308159936706, -2.999999999999971578 ) ) ;
#9184 = DIRECTION ( 'NONE',  ( -1.000000000000000000, 0.000000000000000000, 0.000000000000000000 ) ) ;
#9185 = EDGE_CURVE ( 'NONE', #2945, #17903, #20404, .T. ) ;
#9186 = ORIENTED_EDGE ( 'NONE', *, *, #16859, .T. ) ;
#9187 = ORIENTED_EDGE ( 'NONE', *, *, #18035, .T. ) ;
#9188 = ORIENTED_EDGE ( 'NONE', *, *, #13504, .F. ) ;
#9189 = ORIENTED_EDGE ( 'NONE', *, *, #13218, .T. ) ;
#9190 = CARTESIAN_POINT ( 'NONE',  ( -34.99999999999999289, 0.000000000000000000, -3.012171160963566127E-14 ) ) ;
#9191 = CARTESIAN_POINT ( 'NONE',  ( 48.93401015228426587, 10.00000000000000000, 46.57614213197968667 ) ) ;
#9192 = CARTESIAN_POINT ( 'NONE',  ( 3.997614489231452239, 39.99999999999999289, -51.09533703001513771 ) ) ;
#9193 = DIRECTION ( 'NONE',  ( -1.296372316667914327E-16, -1.000000000000000000, 0.000000000000000000 ) ) ;
#9194 = VERTEX_POINT ( 'NONE', #22379 ) ;
#9195 = DIRECTION ( 'NONE',  ( 0.000000000000000000, -1.000000000000000000, 0.000000000000000000 ) ) ;
#9196 = PLANE ( 'NONE',  #22624 ) ;
#9197 = VERTEX_POINT ( 'NONE', #10206 ) ;
#9198 = CARTESIAN_POINT ( 'NONE',  ( 1.128083539116392364, 34.88850421923958578, -2.999999999999981792 ) ) ;
#9199 = CARTESIAN_POINT ( 'NONE',  ( -11.31876324338254847, -30.07487443287981677, -6.999999999999950262 ) ) ;
#9200 = AXIS2_PLACEMENT_3D ( 'NONE', #15456, #13734, #8379 ) ;
#9201 = LINE ( 'NONE', #14226, #3189 ) ;
#9202 = ORIENTED_EDGE ( 'NONE', *, *, #14699, .F. ) ;
#9203 = DIRECTION ( 'NONE',  ( 0.000000000000000000, 0.000000000000000000, 1.000000000000000000 ) ) ;
#9204 = VERTEX_POINT ( 'NONE', #17198 ) ;
#9205 = CARTESIAN_POINT ( 'NONE',  ( 0.000000000000000000, 30.00000000000000000, -7.500000000000000000 ) ) ;
#9206 = CARTESIAN_POINT ( 'NONE',  ( -4.589505318347434581, 39.46976832855466455, 53.62193830992121235 ) ) ;
#9207 = DIRECTION ( 'NONE',  ( 0.000000000000000000, -1.000000000000000000, 0.000000000000000000 ) ) ;
#9208 = EDGE_LOOP ( 'NONE', ( #13993, #17164, #12395, #19180, #12783, #18344 ) ) ;
#9209 = CARTESIAN_POINT ( 'NONE',  ( 9.952189117650862116, 40.00000000000000000, -53.64426396172072486 ) ) ;
#9210 = CARTESIAN_POINT ( 'NONE',  ( 20.89003165053258826, 11.75591475223826876, 58.31867307082493568 ) ) ;
#9211 = DIRECTION ( 'NONE',  ( -0.000000000000000000, -1.000000000000000000, -0.000000000000000000 ) ) ;
#9212 = EDGE_CURVE ( 'NONE', #20378, #5648, #17470, .T. ) ;
#9213 = EDGE_CURVE ( 'NONE', #159, #20985, #10089, .T. ) ;
#9214 = CARTESIAN_POINT ( 'NONE',  ( 35.00000000000000000, 17.00000000000000000, 39.00000000000003553 ) ) ;
#9215 = ORIENTED_EDGE ( 'NONE', *, *, #7504, .F. ) ;
#9216 = VECTOR ( 'NONE', #22120, 1000.000000000000000 ) ;
#9217 = ORIENTED_EDGE ( 'NONE', *, *, #12124, .F. ) ;
#9218 = EDGE_CURVE ( 'NONE', #14094, #9683, #12325, .T. ) ;
#9219 = ORIENTED_EDGE ( 'NONE', *, *, #19365, .T. ) ;
#9220 = ORIENTED_EDGE ( 'NONE', *, *, #18406, .F. ) ;
#9221 = CARTESIAN_POINT ( 'NONE',  ( -35.00000000000000000, -15.00000000000000000, 2.255140518769849223E-14 ) ) ;
#9222 = CARTESIAN_POINT ( 'NONE',  ( -11.86180952233172725, 39.00000000000000000, -55.35904751184885697 ) ) ;
#9223 = CARTESIAN_POINT ( 'NONE',  ( 35.00000000000000000, -5.000000000000000000, 4.258610482196280173E-15 ) ) ;
#9224 = ORIENTED_EDGE ( 'NONE', *, *, #7839, .T. ) ;
#9225 = CYLINDRICAL_SURFACE ( 'NONE', #3630, 19.11328065563152379 ) ;
#9226 = CARTESIAN_POINT ( 'NONE',  ( 4.238639668822796917E-15, 4.500000000000007105, 0.000000000000000000 ) ) ;
#9227 = VERTEX_POINT ( 'NONE', #7008 ) ;
#9228 = DIRECTION ( 'NONE',  ( -1.000000000000000000, -1.208970125616060717E-17, 0.000000000000000000 ) ) ;
#9229 = DIRECTION ( 'NONE',  ( -0.000000000000000000, -1.000000000000000000, -0.000000000000000000 ) ) ;
#9230 = CARTESIAN_POINT ( 'NONE',  ( -90.00000000000000000, 40.00000000000000000, -2.500000000000003109 ) ) ;
#9231 = SURFACE_STYLE_FILL_AREA ( #5566 ) ;
#9232 = AXIS2_PLACEMENT_3D ( 'NONE', #9459, #5903, #7392 ) ;
#9233 = DIRECTION ( 'NONE',  ( 0.000000000000000000, -1.000000000000000000, 0.000000000000000000 ) ) ;
#9234 = CARTESIAN_POINT ( 'NONE',  ( -8.485281374238564212, 1.499999999999997558, 3.000000000000000000 ) ) ;
#9235 = CARTESIAN_POINT ( 'NONE',  ( -3.171166886497724935, 39.94220484565181550, 51.05051218202238061 ) ) ;
#9236 = CARTESIAN_POINT ( 'NONE',  ( 17.99999999999998579, 20.00000000000000711, -105.0000000000000142 ) ) ;
#9237 = ORIENTED_EDGE ( 'NONE', *, *, #11097, .T. ) ;
#9238 = ORIENTED_EDGE ( 'NONE', *, *, #7625, .T. ) ;
#9239 = ORIENTED_EDGE ( 'NONE', *, *, #9143, .F. ) ;
#9240 = CIRCLE ( 'NONE', #22071, 36.76383501243555685 ) ;
#9241 = DIRECTION ( 'NONE',  ( 1.000000000000000000, -1.296372316667914327E-16, 0.000000000000000000 ) ) ;
#9242 = TOROIDAL_SURFACE ( 'NONE', #22072, 34.90673715956759082, 8.750000000000000000 ) ;
#9243 = CARTESIAN_POINT ( 'NONE',  ( -5.007336801250276359, 0.5949183078238818867, -54.03289733825791075 ) ) ;
#9244 = CIRCLE ( 'NONE', #5967, 57.07106781186551103 ) ;
#9245 = EDGE_CURVE ( 'NONE', #17600, #3953, #5384, .T. ) ;
#9246 = CARTESIAN_POINT ( 'NONE',  ( 3.000000000000000444, 15.20112712106396913, 6.485281374238567764 ) ) ;
#9247 = DIRECTION ( 'NONE',  ( 0.000000000000000000, 0.000000000000000000, 1.000000000000000000 ) ) ;
#9248 = CARTESIAN_POINT ( 'NONE',  ( 12.84899528830093196, 2.142135623730927030, 57.90797000640142045 ) ) ;
#9249 = CARTESIAN_POINT ( 'NONE',  ( -16.09174361829569122, 8.097379805989266544, 59.53987500167126257 ) ) ;
#9250 = CARTESIAN_POINT ( 'NONE',  ( -12.81940492552891797, 35.37234179763732556, -55.76972854553744696 ) ) ;
#9251 = CARTESIAN_POINT ( 'NONE',  ( 25.00000000000000000, -20.00000000000000000, 6.487780019669002523E-15 ) ) ;
#9252 = LINE ( 'NONE', #2623, #9722 ) ;
#9253 = EDGE_CURVE ( 'NONE', #8612, #21119, #21116, .T. ) ;
#9254 = EDGE_CURVE ( 'NONE', #20081, #18060, #4843, .T. ) ;
#9255 = ORIENTED_EDGE ( 'NONE', *, *, #14210, .T. ) ;
#9256 = DIRECTION ( 'NONE',  ( 6.505213034913038160E-19, 3.903127820947822896E-18, 1.000000000000000000 ) ) ;
#9257 = CARTESIAN_POINT ( 'NONE',  ( -1.387778780781445518E-14, 20.00000000000000355, 100.0000000000000000 ) ) ;
#9258 = CARTESIAN_POINT ( 'NONE',  ( -1.255529093608962921, 39.96306425836119303, -50.19904361858059616 ) ) ;
#9259 = DIRECTION ( 'NONE',  ( -0.000000000000000000, 1.000000000000000000, -0.000000000000000000 ) ) ;
#9260 = FACE_OUTER_BOUND ( 'NONE', #10088, .T. ) ;
#9261 = ORIENTED_EDGE ( 'NONE', *, *, #18625, .T. ) ;
#9262 = DIRECTION ( 'NONE',  ( 4.718764931986839378E-35, -3.903127820947822896E-18, -1.000000000000000000 ) ) ;
#9263 = AXIS2_PLACEMENT_3D ( 'NONE', #5904, #12872, #286 ) ;
#9264 = VERTEX_POINT ( 'NONE', #13745 ) ;
#9265 = CARTESIAN_POINT ( 'NONE',  ( 2.775557561562891351E-14, -2.775557561562891351E-14, 2.999999999999999112 ) ) ;
#9266 = CARTESIAN_POINT ( 'NONE',  ( -19.59430950039299546, 28.88846368933323205, 2.999999999999995559 ) ) ;
#9267 = AXIS2_PLACEMENT_3D ( 'NONE', #2271, #16240, #7544 ) ;
#9268 = AXIS2_PLACEMENT_3D ( 'NONE', #9782, #16774, #18720 ) ;
#9269 = CARTESIAN_POINT ( 'NONE',  ( 18.15458487487614647, 6.756534690976822688, -57.58998093367154070 ) ) ;
#9270 = EDGE_CURVE ( 'NONE', #7486, #18033, #3118, .T. ) ;
#9271 = ORIENTED_EDGE ( 'NONE', *, *, #10561, .T. ) ;
#9272 = CARTESIAN_POINT ( 'NONE',  ( -34.88850421923971368, 1.128083539116031542, -2.999999999999981792 ) ) ;
#9273 = AXIS2_PLACEMENT_3D ( 'NONE', #16447, #19885, #756 ) ;
#9274 = DIRECTION ( 'NONE',  ( -0.000000000000000000, -1.000000000000000000, -0.000000000000000000 ) ) ;
#9275 = ADVANCED_FACE ( 'NONE', ( #19490 ), #10642, .F. ) ;
#9276 = ORIENTED_EDGE ( 'NONE', *, *, #13419, .F. ) ;
#9277 = DIRECTION ( 'NONE',  ( 1.296372316667914327E-16, 1.000000000000000000, -0.000000000000000000 ) ) ;
#9278 = CARTESIAN_POINT ( 'NONE',  ( 35.00000000000000000, -9.000000000000001776, 4.258610482196280173E-15 ) ) ;
#9279 = AXIS2_PLACEMENT_3D ( 'NONE', #13203, #16552, #4420 ) ;
#9280 = DIRECTION ( 'NONE',  ( -0.000000000000000000, -0.000000000000000000, -1.000000000000000000 ) ) ;
#9281 = ORIENTED_EDGE ( 'NONE', *, *, #4880, .F. ) ;
#9282 = DIRECTION ( 'NONE',  ( -0.7752116086454780008, 0.5577761202038525878, 0.2965345874457610553 ) ) ;
#9283 = AXIS2_PLACEMENT_3D ( 'NONE', #7920, #20294, #7796 ) ;
#9284 = CARTESIAN_POINT ( 'NONE',  ( -11.00126833625150802, 3.276569432399059512, -57.62199738687990447 ) ) ;
#9285 = VERTEX_POINT ( 'NONE', #17646 ) ;
#9286 = CARTESIAN_POINT ( 'NONE',  ( -21.41958700883256483, -27.56232195404059837, 2.999999999999995559 ) ) ;
#9287 = CARTESIAN_POINT ( 'NONE',  ( -13.74639653023227481, 28.96193690644924246, 2.999999999999995559 ) ) ;
#9288 = AXIS2_PLACEMENT_3D ( 'NONE', #4603, #9633, #14777 ) ;
#9289 = DIRECTION ( 'NONE',  ( 1.000000000000000000, 1.208970125616063182E-17, 0.000000000000000000 ) ) ;
#9290 = EDGE_CURVE ( 'NONE', #15500, #22647, #10130, .T. ) ;
#9291 = CARTESIAN_POINT ( 'NONE',  ( -26.00000000000001421, 19.99999999999982947, 60.00099999999999767 ) ) ;
#9292 = ORIENTED_EDGE ( 'NONE', *, *, #14469, .T. ) ;
#9293 = CARTESIAN_POINT ( 'NONE',  ( -1.387778780781445676E-14, 20.00000000000000000, -105.0020000000000095 ) ) ;
#9294 = CARTESIAN_POINT ( 'NONE',  ( -5.833333333333328596, 33.81926995981417861, 40.61164310337068173 ) ) ;
#9295 = CARTESIAN_POINT ( 'NONE',  ( -4.516278128484037424, 39.87315170859984192, -51.91186101216593585 ) ) ;
#9296 = ORIENTED_EDGE ( 'NONE', *, *, #7650, .F. ) ;
#9297 = CARTESIAN_POINT ( 'NONE',  ( 34.99999999999980815, 28.00000000000000000, 54.99999999999922551 ) ) ;
#9298 = VECTOR ( 'NONE', #16107, 1000.000000000000000 ) ;
#9299 = DIRECTION ( 'NONE',  ( 0.000000000000000000, 0.000000000000000000, -1.000000000000000000 ) ) ;
#9300 = DIRECTION ( 'NONE',  ( -1.000000000000000000, 1.084202172485504434E-16, 0.000000000000000000 ) ) ;
#9301 = VECTOR ( 'NONE', #17978, 1000.000000000000000 ) ;
#9302 = EDGE_CURVE ( 'NONE', #16523, #13978, #15984, .T. ) ;
#9303 = VERTEX_POINT ( 'NONE', #11002 ) ;
#9304 = ORIENTED_EDGE ( 'NONE', *, *, #1067, .T. ) ;
#9305 = EDGE_LOOP ( 'NONE', ( #19417, #21675, #21571 ) ) ;
#9306 =( NAMED_UNIT ( * ) PLANE_ANGLE_UNIT ( ) SI_UNIT ( $, .RADIAN. ) );
#9307 = ADVANCED_FACE ( 'NONE', ( #12822 ), #17990, .F. ) ;
#9308 = ADVANCED_FACE ( 'NONE', ( #1955 ), #14077, .F. ) ;
#9309 = EDGE_LOOP ( 'NONE', ( #20973, #7136, #14241, #3385 ) ) ;
#9310 = DIRECTION ( 'NONE',  ( -0.000000000000000000, 1.000000000000000000, -0.000000000000000000 ) ) ;
#9311 = CARTESIAN_POINT ( 'NONE',  ( 2.854018578421813982E-15, -6.180736333215565814, 0.000000000000000000 ) ) ;
#9312 = LINE ( 'NONE', #255, #7726 ) ;
#9313 = DIRECTION ( 'NONE',  ( -1.000000000000000000, -1.208970125616077665E-17, 0.000000000000000000 ) ) ;
#9314 = AXIS2_PLACEMENT_3D ( 'NONE', #20323, #13187, #20095 ) ;
#9315 = ORIENTED_EDGE ( 'NONE', *, *, #13579, .T. ) ;
#9316 = DIRECTION ( 'NONE',  ( -1.000000000000000000, -1.208970125616060717E-17, 0.000000000000000000 ) ) ;
#9317 = CARTESIAN_POINT ( 'NONE',  ( -31.92986134326219982, 18.22261011550282817, -2.800654218530485018 ) ) ;
#9318 = VERTEX_POINT ( 'NONE', #5614 ) ;
#9319 = DIRECTION ( 'NONE',  ( 1.296372316667914327E-16, 1.000000000000000000, -0.000000000000000000 ) ) ;
#9320 = CARTESIAN_POINT ( 'NONE',  ( -17.96165932904281348, 6.521477064918317801, -57.53061250216237710 ) ) ;
#9321 = CARTESIAN_POINT ( 'NONE',  ( 35.28654656445771565, 4.153516728483715781, 3.000000000000051958 ) ) ;
#9322 = ORIENTED_EDGE ( 'NONE', *, *, #12062, .T. ) ;
#9323 = CARTESIAN_POINT ( 'NONE',  ( -15.50000000000011013, 42.51666049839536043, 100.0000000000000000 ) ) ;
#9324 = ORIENTED_EDGE ( 'NONE', *, *, #2741, .F. ) ;
#9325 = CARTESIAN_POINT ( 'NONE',  ( 9.786525054697406745, 39.51684776735954330, 54.52238233457818239 ) ) ;
#9326 = EDGE_CURVE ( 'NONE', #5303, #3679, #2087, .T. ) ;
#9327 = VECTOR ( 'NONE', #2109, 1000.000000000000000 ) ;
#9328 = CARTESIAN_POINT ( 'NONE',  ( -5.833333333333339255, 39.00000000000000711, -40.61164310337066041 ) ) ;
#9329 = VERTEX_POINT ( 'NONE', #9287 ) ;
#9330 = FACE_OUTER_BOUND ( 'NONE', #12874, .T. ) ;
#9331 = CARTESIAN_POINT ( 'NONE',  ( 12.26943921815721517, 35.80002840870928793, 58.15275698935946735 ) ) ;
#9332 = CARTESIAN_POINT ( 'NONE',  ( 2.775557561562891351E-14, -2.775557561562891351E-14, 2.999999999999999112 ) ) ;
#9333 = EDGE_CURVE ( 'NONE', #13252, #16345, #10881, .T. ) ;
#9334 = CARTESIAN_POINT ( 'NONE',  ( 2.220446049250313081E-13, 2.775557561562891351E-14, -2.800654218530485018 ) ) ;
#9335 = FACE_OUTER_BOUND ( 'NONE', #13954, .T. ) ;
#9336 = EDGE_CURVE ( 'NONE', #21534, #2308, #3956, .T. ) ;
#9337 = AXIS2_PLACEMENT_3D ( 'NONE', #3313, #22335, #8122 ) ;
#9338 = ORIENTED_EDGE ( 'NONE', *, *, #11285, .T. ) ;
#9339 = AXIS2_PLACEMENT_3D ( 'NONE', #7669, #11091, #21536 ) ;
#9340 = VERTEX_POINT ( 'NONE', #9406 ) ;
#9341 = ORIENTED_EDGE ( 'NONE', *, *, #12671, .T. ) ;
#9342 = EDGE_LOOP ( 'NONE', ( #10544, #22673, #11027, #13725 ) ) ;
#9343 = CARTESIAN_POINT ( 'NONE',  ( 35.00000000000000000, -5.000000000000000000, 4.258610482196280173E-15 ) ) ;
#9344 = DIRECTION ( 'NONE',  ( -1.296372316667914327E-16, -1.000000000000000000, 0.000000000000000000 ) ) ;
#9345 = CARTESIAN_POINT ( 'NONE',  ( -15.12081897056664914, 33.51030287062364721, -2.800654218530457484 ) ) ;
#9346 = EDGE_LOOP ( 'NONE', ( #13611, #7975, #9870, #4290, #22205, #9220 ) ) ;
#9347 = CARTESIAN_POINT ( 'NONE',  ( -11.31876324338268880, -30.07487443287981677, 2.999999999999995559 ) ) ;
#9348 = CARTESIAN_POINT ( 'NONE',  ( -8.479740367040006888, -4.901256658985764680, 50.57596245086825348 ) ) ;
#9349 = CIRCLE ( 'NONE', #12255, 2.500000000000002220 ) ;
#9350 = ADVANCED_FACE ( 'NONE', ( #12590 ), #7567, .T. ) ;
#9351 = CIRCLE ( 'NONE', #20697, 19.11328065563151668 ) ;
#9352 = ORIENTED_EDGE ( 'NONE', *, *, #8448, .F. ) ;
#9353 = LINE ( 'NONE', #2361, #8640 ) ;
#9354 = CARTESIAN_POINT ( 'NONE',  ( 42.50000000000000711, -12.00000000000000000, -54.00000000000000000 ) ) ;
#9355 = DIRECTION ( 'NONE',  ( 0.000000000000000000, 0.000000000000000000, 1.000000000000000000 ) ) ;
#9356 = AXIS2_PLACEMENT_3D ( 'NONE', #22267, #15247, #4508 ) ;
#9357 = CARTESIAN_POINT ( 'NONE',  ( 25.00000000000000000, 20.00000000000000000, 6.487780019669002523E-15 ) ) ;
#9358 = CARTESIAN_POINT ( 'NONE',  ( 35.00000000000001421, 5.000000000000000000, 1.540743955509788682E-30 ) ) ;
#9359 = CARTESIAN_POINT ( 'NONE',  ( -34.90673715956725687, 2.728857438001962765E-14, -2.999999999999971578 ) ) ;
#9360 = DIRECTION ( 'NONE',  ( -0.000000000000000000, -1.000000000000000000, -0.000000000000000000 ) ) ;
#9361 = VECTOR ( 'NONE', #17434, 1000.000000000000114 ) ;
#9362 = AXIS2_PLACEMENT_3D ( 'NONE', #3979, #8788, #7058 ) ;
#9363 = EDGE_LOOP ( 'NONE', ( #6049, #4274, #9352, #7388 ) ) ;
#9364 = AXIS2_PLACEMENT_3D ( 'NONE', #2247, #865, #16336 ) ;
#9365 = B_SPLINE_CURVE_WITH_KNOTS ( 'NONE', 3,
 ( #19598, #228, #9165, #12373 ),
 .UNSPECIFIED., .F., .F.,
 ( 4, 4 ),
 ( 0.001893031756885165751, 0.003808480026563545139 ),
 .UNSPECIFIED. ) ;
#9366 = ORIENTED_EDGE ( 'NONE', *, *, #8839, .F. ) ;
#9367 = AXIS2_PLACEMENT_3D ( 'NONE', #3778, #10741, #10861 ) ;
#9368 = ORIENTED_EDGE ( 'NONE', *, *, #16106, .F. ) ;
#9369 = AXIS2_PLACEMENT_3D ( 'NONE', #4567, #18654, #2732 ) ;
#9370 = DIRECTION ( 'NONE',  ( 0.000000000000000000, 0.000000000000000000, -1.000000000000000000 ) ) ;
#9371 = CARTESIAN_POINT ( 'NONE',  ( -42.49999999999996447, 10.00000000000000000, -47.50000000000000711 ) ) ;
#9372 = EDGE_CURVE ( 'NONE', #1931, #8987, #7370, .T. ) ;
#9373 = CARTESIAN_POINT ( 'NONE',  ( -1.788720539129516747E-14, -0.8525878274356358810, 48.47769062749615188 ) ) ;
#9374 = DIRECTION ( 'NONE',  ( -1.000000000000000000, 0.000000000000000000, 0.000000000000000000 ) ) ;
#9375 = CIRCLE ( 'NONE', #20713, 36.76383501243555685 ) ;
#9376 = CIRCLE ( 'NONE', #217, 1.000000000000000888 ) ;
#9377 = CARTESIAN_POINT ( 'NONE',  ( -0.7832251647695825936, 40.00000000000098055, -49.34584158999207659 ) ) ;
#9378 = LINE ( 'NONE', #3694, #12269 ) ;
#9379 = AXIS2_PLACEMENT_3D ( 'NONE', #17314, #13751, #22273 ) ;
#9380 = CARTESIAN_POINT ( 'NONE',  ( 35.00000000000058265, 24.73819270004212356, -55.00000000000076028 ) ) ;
#9381 = CARTESIAN_POINT ( 'NONE',  ( -17.09029715894910950, 27.64365646977276469, -2.999999999999971578 ) ) ;
#9382 = CIRCLE ( 'NONE', #15209, 34.90673715956759082 ) ;
#9383 = ORIENTED_EDGE ( 'NONE', *, *, #22203, .F. ) ;
#9384 = EDGE_CURVE ( 'NONE', #6209, #3991, #19835, .T. ) ;
#9385 = DIRECTION ( 'NONE',  ( -0.000000000000000000, -0.000000000000000000, -1.000000000000000000 ) ) ;
#9386 = FACE_OUTER_BOUND ( 'NONE', #16952, .T. ) ;
#9387 = DIRECTION ( 'NONE',  ( 0.000000000000000000, 0.000000000000000000, 1.000000000000000000 ) ) ;
#9388 = CARTESIAN_POINT ( 'NONE',  ( 0.000000000000000000, 15.00000000000000355, 3.999999999999994671 ) ) ;
#9389 = VERTEX_POINT ( 'NONE', #14424 ) ;
#9390 = EDGE_LOOP ( 'NONE', ( #15698, #21146 ) ) ;
#9391 = DIRECTION ( 'NONE',  ( 0.000000000000000000, 0.000000000000000000, 1.000000000000000000 ) ) ;
#9392 = DIRECTION ( 'NONE',  ( 0.000000000000000000, 1.000000000000000000, 0.000000000000000000 ) ) ;
#9393 = EDGE_CURVE ( 'NONE', #11377, #18399, #20416, .T. ) ;
#9394 = ORIENTED_EDGE ( 'NONE', *, *, #9067, .F. ) ;
#9395 = CARTESIAN_POINT ( 'NONE',  ( -35.00000000000000000, 40.00000000000000000, 1.387778780781445676E-14 ) ) ;
#9396 = EDGE_CURVE ( 'NONE', #9318, #6579, #16742, .T. ) ;
#9397 = CARTESIAN_POINT ( 'NONE',  ( 35.00000000000000000, 40.00000000000000000, -58.99999999999993605 ) ) ;
#9398 = ORIENTED_EDGE ( 'NONE', *, *, #12598, .T. ) ;
#9399 = AXIS2_PLACEMENT_3D ( 'NONE', #1815, #17837, #17719 ) ;
#9400 = CARTESIAN_POINT ( 'NONE',  ( -20.00948735876881202, -24.79619811426206510, -2.999999999999995559 ) ) ;
#9401 = CARTESIAN_POINT ( 'NONE',  ( -22.97438720605730822, 22.98755168577401520, -7.000000000000006217 ) ) ;
#9402 = ORIENTED_EDGE ( 'NONE', *, *, #7644, .T. ) ;
#9403 = DIRECTION ( 'NONE',  ( -6.505213034913038160E-19, -3.903127820947822896E-18, -1.000000000000000000 ) ) ;
#9404 = CARTESIAN_POINT ( 'NONE',  ( 35.00000000000000000, -5.000000000000000000, 54.99999999999698019 ) ) ;
#9405 = ORIENTED_EDGE ( 'NONE', *, *, #10524, .F. ) ;
#9406 = CARTESIAN_POINT ( 'NONE',  ( 35.00000000000002132, 0.000000000000000000, 58.99999999999702993 ) ) ;
#9407 = CARTESIAN_POINT ( 'NONE',  ( -5.233853366103144999, 39.99999999999999289, 51.72875135548209613 ) ) ;
#9408 = DIRECTION ( 'NONE',  ( 0.000000000000000000, 0.000000000000000000, 1.000000000000000000 ) ) ;
#9409 = ORIENTED_EDGE ( 'NONE', *, *, #18428, .F. ) ;
#9410 = CARTESIAN_POINT ( 'NONE',  ( 35.00000000000000000, -9.000000000000001776, 4.258610482196280173E-15 ) ) ;
#9411 = CARTESIAN_POINT ( 'NONE',  ( -35.00000000000000000, -9.000000000000001776, 9.000000000000015987 ) ) ;
#9412 = CARTESIAN_POINT ( 'NONE',  ( -24.24871130596417856, 13.99999999999976197, -2.999999999999999112 ) ) ;
#9413 = CIRCLE ( 'NONE', #15967, 19.11328065563150957 ) ;
#9414 = ORIENTED_EDGE ( 'NONE', *, *, #14031, .F. ) ;
#9415 = CARTESIAN_POINT ( 'NONE',  ( -42.50000000000000711, -5.000000000000000000, 45.40000000000001279 ) ) ;
#9416 = DIRECTION ( 'NONE',  ( 1.000000000000000000, 0.000000000000000000, 0.000000000000000000 ) ) ;
#9417 = ORIENTED_EDGE ( 'NONE', *, *, #19831, .F. ) ;
#9418 = ADVANCED_FACE ( 'NONE', ( #5854 ), #19731, .T. ) ;
#9419 = AXIS2_PLACEMENT_3D ( 'NONE', #8271, #15241, #22262 ) ;
#9420 = ORIENTED_EDGE ( 'NONE', *, *, #11112, .F. ) ;
#9421 = B_SPLINE_CURVE_WITH_KNOTS ( 'NONE', 3,
 ( #10146, #13918, #1686, #10370 ),
 .UNSPECIFIED., .F., .F.,
 ( 4, 4 ),
 ( 9.715086407230427146E-07, 0.001929643240672483445 ),
 .UNSPECIFIED. ) ;
#9422 = VERTEX_POINT ( 'NONE', #7340 ) ;
#9423 = AXIS2_PLACEMENT_3D ( 'NONE', #2748, #9274, #566 ) ;
#9424 = ORIENTED_EDGE ( 'NONE', *, *, #10161, .F. ) ;
#9425 = CARTESIAN_POINT ( 'NONE',  ( 11.08851315719092057, 40.00000000000000000, 54.00022650832064386 ) ) ;
#9426 = DIRECTION ( 'NONE',  ( 0.000000000000000000, -1.000000000000000000, 0.000000000000000000 ) ) ;
#9427 = DIRECTION ( 'NONE',  ( 0.000000000000000000, 0.000000000000000000, -1.000000000000000000 ) ) ;
#9428 = DIRECTION ( 'NONE',  ( 1.000000000000000000, 0.000000000000000000, 0.000000000000000000 ) ) ;
#9429 = CARTESIAN_POINT ( 'NONE',  ( 35.00000000000000000, 17.00000000000000000, 41.00000000000002132 ) ) ;
#9430 = ORIENTED_EDGE ( 'NONE', *, *, #18211, .F. ) ;
#9431 = DIRECTION ( 'NONE',  ( 6.505213034913038160E-19, 3.903127820947822896E-18, 1.000000000000000000 ) ) ;
#9432 = DIRECTION ( 'NONE',  ( 1.000000000000000000, 0.000000000000000000, 0.000000000000000000 ) ) ;
#9433 = ORIENTED_EDGE ( 'NONE', *, *, #8740, .T. ) ;
#9434 = CARTESIAN_POINT ( 'NONE',  ( 0.3475255461657534850, -0.009191383995502665563, 50.24722912075116454 ) ) ;
#9435 = DIRECTION ( 'NONE',  ( 1.000000000000000000, 1.208970125616053475E-17, 0.000000000000000000 ) ) ;
#9436 = CARTESIAN_POINT ( 'NONE',  ( 16.09174361829564504, 8.097379805989254109, -59.53987500167121993 ) ) ;
#9437 = ORIENTED_EDGE ( 'NONE', *, *, #4516, .F. ) ;
#9438 = DIRECTION ( 'NONE',  ( -1.000000000000000000, 0.000000000000000000, 0.000000000000000000 ) ) ;
#9439 = EDGE_CURVE ( 'NONE', #15365, #13797, #19687, .T. ) ;
#9440 = CARTESIAN_POINT ( 'NONE',  ( 1.801771875243787013, 0.06844342149310433943, 51.82845797839667767 ) ) ;
#9441 = AXIS2_PLACEMENT_3D ( 'NONE', #5878, #4160, #9428 ) ;
#9442 = ORIENTED_EDGE ( 'NONE', *, *, #7223, .T. ) ;
#9443 = CARTESIAN_POINT ( 'NONE',  ( 5.905661774832184463, 39.12131255383282991, 53.51378690820485673 ) ) ;
#9444 = CIRCLE ( 'NONE', #2489, 36.76383501243555685 ) ;
#9445 = CARTESIAN_POINT ( 'NONE',  ( 4.724946350300523916E-15, 8.251288694035745053, 0.000000000000000000 ) ) ;
#9446 = ORIENTED_EDGE ( 'NONE', *, *, #4273, .F. ) ;
#9447 = AXIS2_PLACEMENT_3D ( 'NONE', #6751, #10393, #10174 ) ;
#9448 = VECTOR ( 'NONE', #9063, 1000.000000000000000 ) ;
#9449 = CARTESIAN_POINT ( 'NONE',  ( -42.50000000000000000, 10.00000000000000000, 47.49999999999999289 ) ) ;
#9450 = DIRECTION ( 'NONE',  ( -0.000000000000000000, -0.000000000000000000, -1.000000000000000000 ) ) ;
#9451 = EDGE_CURVE ( 'NONE', #12869, #626, #20061, .T. ) ;
#9452 = AXIS2_PLACEMENT_3D ( 'NONE', #1822, #15774, #7075 ) ;
#9453 = CARTESIAN_POINT ( 'NONE',  ( 12.99999999999993960, 42.51666049839543149, -105.0000000000000142 ) ) ;
#9454 = EDGE_LOOP ( 'NONE', ( #12266, #22168, #5975, #14521 ) ) ;
#9455 = EDGE_LOOP ( 'NONE', ( #13776, #5692, #18644 ) ) ;
#9456 = CIRCLE ( 'NONE', #5786, 36.76383501243555685 ) ;
#9457 = VERTEX_POINT ( 'NONE', #1032 ) ;
#9458 = ORIENTED_EDGE ( 'NONE', *, *, #18151, .T. ) ;
#9459 = CARTESIAN_POINT ( 'NONE',  ( 42.50000000000000711, -12.00000000000012434, 47.50000000000000711 ) ) ;
#9460 = AXIS2_PLACEMENT_3D ( 'NONE', #4869, #4650, #9681 ) ;
#9461 = CARTESIAN_POINT ( 'NONE',  ( -11.69583325982488908, 39.02781355213843995, -55.28967510482120673 ) ) ;
#9462 = AXIS2_PLACEMENT_3D ( 'NONE', #22093, #16579, #11191 ) ;
#9463 = CARTESIAN_POINT ( 'NONE',  ( 34.99999999999980815, 26.00000000000000355, 54.99999999999922551 ) ) ;
#9464 = AXIS2_PLACEMENT_3D ( 'NONE', #10950, #9005, #298 ) ;
#9465 = ORIENTED_EDGE ( 'NONE', *, *, #5139, .T. ) ;
#9466 = FACE_OUTER_BOUND ( 'NONE', #1661, .T. ) ;
#9467 = CARTESIAN_POINT ( 'NONE',  ( -33.52953626616031357, -9.708269511265493534, 3.000000000000016431 ) ) ;
#9468 = CIRCLE ( 'NONE', #3976, 10.00000000000000000 ) ;
#9469 = EDGE_CURVE ( 'NONE', #573, #260, #11681, .T. ) ;
#9470 = ORIENTED_EDGE ( 'NONE', *, *, #6010, .T. ) ;
#9471 = CARTESIAN_POINT ( 'NONE',  ( 12.24744603030438839, 40.00000000000000000, -54.43639671998947449 ) ) ;
#9472 = CYLINDRICAL_SURFACE ( 'NONE', #18609, 2.500000000000002220 ) ;
#9473 = PLANE ( 'NONE',  #22310 ) ;
#9474 = CARTESIAN_POINT ( 'NONE',  ( -35.00000000000000000, -9.000000000000001776, 1.387778780781445676E-14 ) ) ;
#9475 = CONICAL_SURFACE ( 'NONE', #3996, 9.000000000000035527, 0.7853981633974447263 ) ;
#9476 = EDGE_CURVE ( 'NONE', #5386, #13427, #2533, .T. ) ;
#9477 = EDGE_CURVE ( 'NONE', #14267, #12299, #12704, .T. ) ;
#9478 = VECTOR ( 'NONE', #2356, 1000.000000000000000 ) ;
#9479 = CARTESIAN_POINT ( 'NONE',  ( 17.99999999999998579, 20.00000000000000711, -102.0000000000000142 ) ) ;
#9480 = CARTESIAN_POINT ( 'NONE',  ( 22.26748298433284390, -22.28024240313525439, -6.999999999999950262 ) ) ;
#9481 = AXIS2_PLACEMENT_3D ( 'NONE', #3348, #8489, #22484 ) ;
#9482 = ORIENTED_EDGE ( 'NONE', *, *, #6271, .F. ) ;
#9483 = ORIENTED_EDGE ( 'NONE', *, *, #6684, .F. ) ;
#9484 = EDGE_CURVE ( 'NONE', #8190, #1985, #5960, .T. ) ;
#9485 = ORIENTED_EDGE ( 'NONE', *, *, #15882, .F. ) ;
#9486 = DIRECTION ( 'NONE',  ( 0.000000000000000000, 0.000000000000000000, 1.000000000000000000 ) ) ;
#9487 = MECHANICAL_DESIGN_GEOMETRIC_PRESENTATION_REPRESENTATION (  '', ( #9844 ), #2900 ) ;
#9488 = AXIS2_PLACEMENT_3D ( 'NONE', #9976, #21926, #16969 ) ;
#9489 = DIRECTION ( 'NONE',  ( 0.000000000000000000, 0.7071067811865474617, 0.7071067811865474617 ) ) ;
#9490 = CARTESIAN_POINT ( 'NONE',  ( 7.416183817405959028E-14, -1.031411640100015070, 48.34207013941295372 ) ) ;
#9491 = DIRECTION ( 'NONE',  ( 1.000000000000000000, -0.000000000000000000, -0.000000000000000000 ) ) ;
#9492 = CARTESIAN_POINT ( 'NONE',  ( -9.375585286557477360, 39.53990934012379910, -54.37755512015218784 ) ) ;
#9493 = DIRECTION ( 'NONE',  ( -0.000000000000000000, 1.000000000000000000, -0.000000000000000000 ) ) ;
#9494 = CARTESIAN_POINT ( 'NONE',  ( -34.99999999999998579, -5.000000000000000000, -58.99999999999703704 ) ) ;
#9495 = PRODUCT_DEFINITION_SHAPE ( 'NONE', 'NONE',  #22698 ) ;
#9496 = ORIENTED_EDGE ( 'NONE', *, *, #1518, .F. ) ;
#9497 = CARTESIAN_POINT ( 'NONE',  ( -34.99999999999980815, 40.00000000000000000, 52.89999999999922409 ) ) ;
#9498 = DIRECTION ( 'NONE',  ( -0.000000000000000000, -0.000000000000000000, -1.000000000000000000 ) ) ;
#9499 = CARTESIAN_POINT ( 'NONE',  ( 4.044183821322609990E-15, 3.000000000000006217, 0.000000000000000000 ) ) ;
#9500 = DIRECTION ( 'NONE',  ( 6.505213034913038160E-19, 3.903127820947822896E-18, 1.000000000000000000 ) ) ;
#9501 = VERTEX_POINT ( 'NONE', #16384 ) ;
#9502 = ORIENTED_EDGE ( 'NONE', *, *, #2249, .F. ) ;
#9503 = AXIS2_PLACEMENT_3D ( 'NONE', #16585, #21409, #895 ) ;
#9504 = CARTESIAN_POINT ( 'NONE',  ( -24.75236754129142724, -27.84804035626062202, -2.999999999999971578 ) ) ;
#9505 = CARTESIAN_POINT ( 'NONE',  ( 2.775557561562891351E-14, -2.775557561562891351E-14, 2.999999999999999112 ) ) ;
#9506 = EDGE_CURVE ( 'NONE', #13932, #8686, #15639, .T. ) ;
#9507 = ADVANCED_FACE ( 'NONE', ( #18221 ), #20169, .T. ) ;
#9508 = ORIENTED_EDGE ( 'NONE', *, *, #9724, .T. ) ;
#9509 = DIRECTION ( 'NONE',  ( 0.000000000000000000, 1.000000000000000000, 0.000000000000000000 ) ) ;
#9510 = EDGE_CURVE ( 'NONE', #2931, #10113, #3215, .T. ) ;
#9511 = CARTESIAN_POINT ( 'NONE',  ( 7.434579289837093263, 39.99999999999999289, -52.73242323840388934 ) ) ;
#9512 = EDGE_LOOP ( 'NONE', ( #22215, #13171, #4751, #4738, #11045, #11251 ) ) ;
#9513 = CARTESIAN_POINT ( 'NONE',  ( 3.946564805737537984, 39.90443716270423380, -51.55060807443248194 ) ) ;
#9514 = DIRECTION ( 'NONE',  ( -1.000000000000000000, 9.802091999852178833E-15, 0.000000000000000000 ) ) ;
#9515 = AXIS2_PLACEMENT_3D ( 'NONE', #8450, #1346, #6733 ) ;
#9516 = ORIENTED_EDGE ( 'NONE', *, *, #12978, .F. ) ;
#9517 = CARTESIAN_POINT ( 'NONE',  ( -27.64365646977275048, -17.09029715894938661, -6.999999999999950262 ) ) ;
#9518 = CARTESIAN_POINT ( 'NONE',  ( 10.07716038307521345, 39.27871711258762133, -54.68297691365300039 ) ) ;
#9519 = DIRECTION ( 'NONE',  ( 6.505213034913038160E-19, 3.903127820947822896E-18, 1.000000000000000000 ) ) ;
#9520 = CARTESIAN_POINT ( 'NONE',  ( -10.00000000000000888, 2.999999999999836131, -4.999999999999948486 ) ) ;
#9521 = ORIENTED_EDGE ( 'NONE', *, *, #9794, .T. ) ;
#9522 = DIRECTION ( 'NONE',  ( 0.000000000000000000, 0.000000000000000000, 1.000000000000000000 ) ) ;
#9523 = DIRECTION ( 'NONE',  ( 0.000000000000000000, -1.000000000000000000, 0.000000000000000000 ) ) ;
#9524 = DIRECTION ( 'NONE',  ( 0.000000000000000000, 0.000000000000000000, 1.000000000000000000 ) ) ;
#9525 = EDGE_LOOP ( 'NONE', ( #1259, #22319, #6801, #17381 ) ) ;
#9526 = EDGE_CURVE ( 'NONE', #5633, #6950, #699, .T. ) ;
#9527 = AXIS2_PLACEMENT_3D ( 'NONE', #9278, #8826, #16260 ) ;
#9528 = LINE ( 'NONE', #19257, #2344 ) ;
#9529 = ORIENTED_EDGE ( 'NONE', *, *, #15050, .T. ) ;
#9530 = ORIENTED_EDGE ( 'NONE', *, *, #2014, .F. ) ;
#9531 = ORIENTED_EDGE ( 'NONE', *, *, #9970, .T. ) ;
#9532 =( NAMED_UNIT ( * ) SI_UNIT ( $, .STERADIAN. ) SOLID_ANGLE_UNIT ( ) );
#9533 = ORIENTED_EDGE ( 'NONE', *, *, #6235, .T. ) ;
#9534 = CARTESIAN_POINT ( 'NONE',  ( 9.952189117650823036, 40.00000000000000000, 53.64426396172073197 ) ) ;
#9535 = CARTESIAN_POINT ( 'NONE',  ( 8.460114887479386780, -4.900635315004578274, 50.56657553898163115 ) ) ;
#9536 = VECTOR ( 'NONE', #22304, 1000.000000000000000 ) ;
#9537 = CARTESIAN_POINT ( 'NONE',  ( -8.999999999999952038, 0.000000000000000000, -4.999999999999997335 ) ) ;
#9538 = CARTESIAN_POINT ( 'NONE',  ( 15.50000000000024336, -2.516660498395250745, 105.0000000000000142 ) ) ;
#9539 = CARTESIAN_POINT ( 'NONE',  ( -18.00000000000001421, 20.00000000000000711, 103.0000000000000284 ) ) ;
#9540 = ORIENTED_EDGE ( 'NONE', *, *, #8890, .F. ) ;
#9541 = DIRECTION ( 'NONE',  ( 1.000000000000000000, -1.084202172485504927E-16, 0.000000000000000000 ) ) ;
#9542 = DIRECTION ( 'NONE',  ( -0.000000000000000000, 1.000000000000000000, -0.000000000000000000 ) ) ;
#9543 = EDGE_LOOP ( 'NONE', ( #18859, #12253, #1792, #12098 ) ) ;
#9544 = DIRECTION ( 'NONE',  ( -6.505213034913038160E-19, -3.903127820947822896E-18, -1.000000000000000000 ) ) ;
#9545 = EDGE_CURVE ( 'NONE', #1795, #22114, #7220, .T. ) ;
#9546 = DIRECTION ( 'NONE',  ( -6.505213034913038160E-19, -3.903127820947822896E-18, -1.000000000000000000 ) ) ;
#9547 = CARTESIAN_POINT ( 'NONE',  ( 11.68090480754629112, 3.765577839755377187, -57.90797000640139913 ) ) ;
#9548 = ORIENTED_EDGE ( 'NONE', *, *, #5522, .T. ) ;
#9549 = DIRECTION ( 'NONE',  ( -0.000000000000000000, -1.000000000000000000, -0.000000000000000000 ) ) ;
#9550 = ORIENTED_EDGE ( 'NONE', *, *, #13041, .T. ) ;
#9551 = CARTESIAN_POINT ( 'NONE',  ( 7.073804381388024254, 38.72385617084731280, 54.13593115560357205 ) ) ;
#9552 = CARTESIAN_POINT ( 'NONE',  ( -7.882609639814679786E-15, -9.552912840896525389E-26, -50.50395615645409464 ) ) ;
#9553 = ORIENTED_EDGE ( 'NONE', *, *, #14038, .F. ) ;
#9554 = DIRECTION ( 'NONE',  ( -6.505213034913038160E-19, -3.903127820947822896E-18, -1.000000000000000000 ) ) ;
#9555 = EDGE_CURVE ( 'NONE', #8509, #9389, #20286, .T. ) ;
#9556 = CARTESIAN_POINT ( 'NONE',  ( 17.16827611621489424, 34.47540479398339386, 57.28984973304910255 ) ) ;
#9557 = CIRCLE ( 'NONE', #19796, 41.00000000000000000 ) ;
#9558 = CIRCLE ( 'NONE', #1132, 15.00000000000000000 ) ;
#9559 = FACE_OUTER_BOUND ( 'NONE', #7867, .T. ) ;
#9560 = ORIENTED_EDGE ( 'NONE', *, *, #6261, .F. ) ;
#9561 = EDGE_LOOP ( 'NONE', ( #14433, #8681, #9402, #1211 ) ) ;
#9562 = EDGE_CURVE ( 'NONE', #478, #13151, #9564, .T. ) ;
#9563 = ORIENTED_EDGE ( 'NONE', *, *, #18444, .F. ) ;
#9564 = B_SPLINE_CURVE_WITH_KNOTS ( 'NONE', 3,
 ( #11452, #9855, #9518, #16843, #18440, #18558, #18329, #9737, #1142, #4589, #16724, #14872, #8135 ),
 .UNSPECIFIED., .F., .F.,
 ( 4, 2, 1, 1, 1, 2, 2, 4 ),
 ( 0.000000000000000000, 0.2499999999999895639, 0.3749999999999843459, 0.4374999999999821809, 0.4687499999999784617, 0.4843749999999783507, 0.4999999999999782396, 1.000000000000000000 ),
 .UNSPECIFIED. ) ;
#9565 = ORIENTED_EDGE ( 'NONE', *, *, #6995, .F. ) ;
#9566 = CARTESIAN_POINT ( 'NONE',  ( 26.65040777864179944, 24.43568323314229929, 2.932460736555799752 ) ) ;
#9567 = FACE_OUTER_BOUND ( 'NONE', #3832, .T. ) ;
#9568 = ORIENTED_EDGE ( 'NONE', *, *, #16859, .F. ) ;
#9569 = CARTESIAN_POINT ( 'NONE',  ( 1.423424233832903951, 32.35999952201579077, 3.000000000000002665 ) ) ;
#9570 = CARTESIAN_POINT ( 'NONE',  ( 0.002911692990617354218, 40.00000000000000711, 48.73623850383051348 ) ) ;
#9571 = VERTEX_POINT ( 'NONE', #21663 ) ;
#9572 = ADVANCED_FACE ( 'NONE', ( #6075 ), #15992, .F. ) ;
#9573 = ORIENTED_EDGE ( 'NONE', *, *, #3565, .T. ) ;
#9574 = DIRECTION ( 'NONE',  ( 6.505213034913038160E-19, 3.903127820947822896E-18, 1.000000000000000000 ) ) ;
#9575 = DIRECTION ( 'NONE',  ( 0.000000000000000000, 0.000000000000000000, 1.000000000000000000 ) ) ;
#9576 = CARTESIAN_POINT ( 'NONE',  ( 3.330669073875469621E-13, -1.110223024625156540E-13, -2.999999999999971578 ) ) ;
#9577 = CARTESIAN_POINT ( 'NONE',  ( 25.00000000000000000, 20.00000000000000000, 6.487780019669002523E-15 ) ) ;
#9578 = CONICAL_SURFACE ( 'NONE', #22401, 2.524999999999999467, 0.7853981633974482790 ) ;
#9579 = DIRECTION ( 'NONE',  ( 1.296372316667914327E-16, 1.000000000000000000, -0.000000000000000000 ) ) ;
#9580 = DIRECTION ( 'NONE',  ( 0.000000000000000000, -1.000000000000000000, 0.000000000000000000 ) ) ;
#9581 = VERTEX_POINT ( 'NONE', #7083 ) ;
#9582 = VERTEX_POINT ( 'NONE', #323 ) ;
#9583 = EDGE_CURVE ( 'NONE', #11088, #13179, #17851, .T. ) ;
#9584 = ORIENTED_EDGE ( 'NONE', *, *, #2365, .T. ) ;
#9585 = CARTESIAN_POINT ( 'NONE',  ( -18.14868794606802282, 11.58103667096326639, 57.62894917896124980 ) ) ;
#9586 = DIRECTION ( 'NONE',  ( -0.000000000000000000, 1.000000000000000000, -0.000000000000000000 ) ) ;
#9587 = DIRECTION ( 'NONE',  ( -6.505213034913038160E-19, -3.903127820947822896E-18, -1.000000000000000000 ) ) ;
#9588 = EDGE_CURVE ( 'NONE', #21565, #8405, #5372, .T. ) ;
#9589 = CIRCLE ( 'NONE', #8496, 16.99999999999998579 ) ;
#9590 = DIRECTION ( 'NONE',  ( 0.000000000000000000, 1.000000000000000000, 0.000000000000000000 ) ) ;
#9591 = CARTESIAN_POINT ( 'NONE',  ( -4.295527433237782828E-15, -1.236374842841486021, 48.24164917503448180 ) ) ;
#9592 = CARTESIAN_POINT ( 'NONE',  ( 18.42595423422130452, -0.9047447100419843125, 2.256528587417473578E-15 ) ) ;
#9593 = FACE_OUTER_BOUND ( 'NONE', #16380, .T. ) ;
#9594 = DIRECTION ( 'NONE',  ( -1.000000000000000000, 0.000000000000000000, 0.000000000000000000 ) ) ;
#9595 = DIRECTION ( 'NONE',  ( -1.000000000000000000, -1.208970125616046080E-17, 6.505213034913038160E-19 ) ) ;
#9596 = ORIENTED_EDGE ( 'NONE', *, *, #19541, .F. ) ;
#9597 = DIRECTION ( 'NONE',  ( -0.000000000000000000, 1.000000000000000000, -0.000000000000000000 ) ) ;
#9598 = EDGE_CURVE ( 'NONE', #1297, #5408, #13634, .T. ) ;
#9599 = CARTESIAN_POINT ( 'NONE',  ( 5.761125704852336857E-15, -0.9047447100419790944, -18.42595423422130452 ) ) ;
#9600 = DIRECTION ( 'NONE',  ( 0.000000000000000000, 0.7071067811865507924, 0.7071067811865441310 ) ) ;
#9601 = LINE ( 'NONE', #16587, #15856 ) ;
#9602 = ORIENTED_EDGE ( 'NONE', *, *, #12811, .T. ) ;
#9603 = DIRECTION ( 'NONE',  ( -1.000000000000000000, -1.208970125616062874E-17, 0.000000000000000000 ) ) ;
#9604 = EDGE_LOOP ( 'NONE', ( #2152, #6198 ) ) ;
#9605 = LINE ( 'NONE', #21995, #18088 ) ;
#9606 = CARTESIAN_POINT ( 'NONE',  ( 35.00000000000000000, 0.000000000000000000, 57.49999999999698730 ) ) ;
#9607 = ADVANCED_FACE ( 'NONE', ( #1929 ), #8912, .T. ) ;
#9608 = EDGE_CURVE ( 'NONE', #8022, #16638, #5483, .T. ) ;
#9609 = VERTEX_POINT ( 'NONE', #10731 ) ;
#9610 = AXIS2_PLACEMENT_3D ( 'NONE', #15257, #6341, #844 ) ;
#9611 = DIRECTION ( 'NONE',  ( 1.000000000000000000, 0.000000000000000000, 0.000000000000000000 ) ) ;
#9612 = CARTESIAN_POINT ( 'NONE',  ( 5.188165876950928457, 39.99999999999999289, -51.70385275873069020 ) ) ;
#9613 = ORIENTED_EDGE ( 'NONE', *, *, #16512, .T. ) ;
#9614 = CARTESIAN_POINT ( 'NONE',  ( 2.999999999999997780, 15.99999999999999645, 8.485281374238567764 ) ) ;
#9615 = CARTESIAN_POINT ( 'NONE',  ( 12.24744603029285273, 40.00000000000000000, 54.43639671998466412 ) ) ;
#9616 = CARTESIAN_POINT ( 'NONE',  ( -8.256135806682724620, -0.3920627093389371653, 55.63523492904089096 ) ) ;
#9617 = CARTESIAN_POINT ( 'NONE',  ( -26.64365646977265456, -17.09029715894938661, -2.999999999999981792 ) ) ;
#9618 = CARTESIAN_POINT ( 'NONE',  ( -14.31754202316403735, 5.927758996452408446, -58.94936959136224885 ) ) ;
#9619 = EDGE_CURVE ( 'NONE', #14924, #2722, #427, .T. ) ;
#9620 = CARTESIAN_POINT ( 'NONE',  ( -9.727693426874370886, 39.99999999999998579, 53.57919861644133874 ) ) ;
#9621 = ADVANCED_FACE ( 'NONE', ( #9593 ), #20691, .F. ) ;
#9622 = AXIS2_PLACEMENT_3D ( 'NONE', #13569, #20581, #4443 ) ;
#9623 = DIRECTION ( 'NONE',  ( -0.000000000000000000, 1.000000000000000000, -0.000000000000000000 ) ) ;
#9624 = ORIENTED_EDGE ( 'NONE', *, *, #17951, .F. ) ;
#9625 = CARTESIAN_POINT ( 'NONE',  ( 24.03323817228489290, -20.36304159388394197, -7.000000000000006217 ) ) ;
#9626 = CARTESIAN_POINT ( 'NONE',  ( -12.24744603030441148, 40.00000000000000000, 54.43639671998950291 ) ) ;
#9627 = CARTESIAN_POINT ( 'NONE',  ( -31.41239365194207878, 2.347663744114270035, 3.000000000000023537 ) ) ;
#9628 = AXIS2_PLACEMENT_3D ( 'NONE', #5749, #18114, #7465 ) ;
#9629 = ORIENTED_EDGE ( 'NONE', *, *, #4570, .F. ) ;
#9630 = CARTESIAN_POINT ( 'NONE',  ( 9.103081159015365742, 0.03030367950460663429, 53.87333532811653214 ) ) ;
#9631 = ADVANCED_FACE ( 'NONE', ( #11193 ), #5394, .T. ) ;
#9632 = CARTESIAN_POINT ( 'NONE',  ( -10.63866000424708247, 30.58060543830997702, 43.66469350997160603 ) ) ;
#9633 = DIRECTION ( 'NONE',  ( -6.505213034913038160E-19, -3.903127820947822896E-18, -1.000000000000000000 ) ) ;
#9634 = AXIS2_PLACEMENT_3D ( 'NONE', #11166, #2478, #7629 ) ;
#9635 = ORIENTED_EDGE ( 'NONE', *, *, #20140, .F. ) ;
#9636 = AXIS2_PLACEMENT_3D ( 'NONE', #15074, #784, #19918 ) ;
#9637 = ORIENTED_EDGE ( 'NONE', *, *, #4711, .F. ) ;
#9638 = AXIS2_PLACEMENT_3D ( 'NONE', #5490, #12572, #3674 ) ;
#9639 = DIRECTION ( 'NONE',  ( 0.9898482782746246267, -0.1420899137197702278, 0.003292782390244445006 ) ) ;
#9640 = VECTOR ( 'NONE', #4933, 1000.000000000000114 ) ;
#9641 = EDGE_LOOP ( 'NONE', ( #3524, #7249, #20475, #21950 ) ) ;
#9642 = FACE_BOUND ( 'NONE', #3238, .T. ) ;
#9643 = CARTESIAN_POINT ( 'NONE',  ( -11.93972437435557232, -29.14949368109881433, -2.999999999999971578 ) ) ;
#9644 = CARTESIAN_POINT ( 'NONE',  ( 6.383438919230843859E-14, 1.500000000000015099, -20.00000000000029488 ) ) ;
#9645 = CYLINDRICAL_SURFACE ( 'NONE', #2947, 49.99999999999998579 ) ;
#9646 = CARTESIAN_POINT ( 'NONE',  ( -27.01645732367859054, -17.86915608785693976, -2.999999999999999112 ) ) ;
#9647 = VERTEX_POINT ( 'NONE', #780 ) ;
#9648 = CARTESIAN_POINT ( 'NONE',  ( 24.62019382530525391, -4.341204441673101933, -2.999999999999999112 ) ) ;
#9649 = FACE_OUTER_BOUND ( 'NONE', #10571, .T. ) ;
#9650 = EDGE_LOOP ( 'NONE', ( #10276, #8601, #5144, #15479 ) ) ;
#9651 = CARTESIAN_POINT ( 'NONE',  ( -14.92530643917655730, 18.45549920837825653, -45.79309713780077828 ) ) ;
#9652 = EDGE_CURVE ( 'NONE', #21024, #21115, #11997, .T. ) ;
#9653 = CARTESIAN_POINT ( 'NONE',  ( -14.98269809772828864, 3.197274675470663574, -56.58282704237542760 ) ) ;
#9654 = CIRCLE ( 'NONE', #14808, 34.90673715956759082 ) ;
#9655 = CARTESIAN_POINT ( 'NONE',  ( 9.689843208404433028, 39.33333333333334991, 54.54983754392749518 ) ) ;
#9656 = ORIENTED_EDGE ( 'NONE', *, *, #3871, .F. ) ;
#9657 = CARTESIAN_POINT ( 'NONE',  ( -0.7785680137044753701, 40.00000000000002842, -49.23936450072109494 ) ) ;
#9658 = DIRECTION ( 'NONE',  ( 0.000000000000000000, 1.000000000000000000, 0.000000000000000000 ) ) ;
#9659 = EDGE_LOOP ( 'NONE', ( #21951, #10672, #1685, #17825 ) ) ;
#9660 = CARTESIAN_POINT ( 'NONE',  ( 90.00000000000000000, 24.73819270004212356, -9.108981535246192915E-16 ) ) ;
#9661 = CARTESIAN_POINT ( 'NONE',  ( 10.49999999999994138, 42.51666049839543149, 105.0000000000000142 ) ) ;
#9662 = CARTESIAN_POINT ( 'NONE',  ( -1.145641935386710886, 0.005153623471255848118, -49.65547338460926596 ) ) ;
#9663 = ORIENTED_EDGE ( 'NONE', *, *, #18719, .T. ) ;
#9664 = DIRECTION ( 'NONE',  ( -0.000000000000000000, -0.000000000000000000, -1.000000000000000000 ) ) ;
#9665 = UNCERTAINTY_MEASURE_WITH_UNIT (LENGTH_MEASURE( 1.000000000000000082E-05 ), #9869, 'distance_accuracy_value', 'NONE');
#9666 = CARTESIAN_POINT ( 'NONE',  ( 13.25803659942245538, 34.99815359651562119, 58.54720450724165204 ) ) ;
#9667 = LINE ( 'NONE', #21944, #16951 ) ;
#9668 = CARTESIAN_POINT ( 'NONE',  ( 31.21605069118088593, 8.646032897228984382, -2.999999999999999112 ) ) ;
#9669 = CARTESIAN_POINT ( 'NONE',  ( 17.41694144196580396, 10.15895996405146029, -59.94253659024143843 ) ) ;
#9670 = B_SPLINE_CURVE_WITH_KNOTS ( 'NONE', 3,
 ( #11029, #18016, #2787, #2327 ),
 .UNSPECIFIED., .F., .F.,
 ( 4, 4 ),
 ( 0.001875451646902858305, 0.003761979286331158800 ),
 .UNSPECIFIED. ) ;
#9672 = ORIENTED_EDGE ( 'NONE', *, *, #16557, .T. ) ;
#9671 = EDGE_CURVE ( 'NONE', #7701, #8965, #4319, .T. ) ;
#9673 = ORIENTED_EDGE ( 'NONE', *, *, #10603, .T. ) ;
#9674 = CIRCLE ( 'NONE', #3081, 18.00000000000000000 ) ;
#9675 = EDGE_LOOP ( 'NONE', ( #3577, #13696, #1672, #14952 ) ) ;
#9676 = EDGE_LOOP ( 'NONE', ( #12787, #11279, #9790, #11955, #15254, #8076 ) ) ;
#9677 = LINE ( 'NONE', #18622, #12883 ) ;
#9678 = ADVANCED_FACE ( 'NONE', ( #18304 ), #18759, .F. ) ;
#9679 = CONICAL_SURFACE ( 'NONE', #4919, 58.99999999999994316, 0.7853981633974725929 ) ;
#9680 = VERTEX_POINT ( 'NONE', #13689 ) ;
#9681 = DIRECTION ( 'NONE',  ( 0.000000000000000000, 0.000000000000000000, 1.000000000000000000 ) ) ;
#9682 = DIRECTION ( 'NONE',  ( 0.000000000000000000, 1.000000000000000000, 0.000000000000000000 ) ) ;
#9683 = VERTEX_POINT ( 'NONE', #22431 ) ;
#9684 = DIRECTION ( 'NONE',  ( -1.000000000000000000, -1.208970125616057944E-17, 0.000000000000000000 ) ) ;
#9685 = AXIS2_PLACEMENT_3D ( 'NONE', #15370, #15710, #1408 ) ;
#9686 = ORIENTED_EDGE ( 'NONE', *, *, #1484, .T. ) ;
#9687 = DIRECTION ( 'NONE',  ( 0.000000000000000000, 0.000000000000000000, -1.000000000000000000 ) ) ;
#9688 = CYLINDRICAL_SURFACE ( 'NONE', #21151, 2.099999999999997868 ) ;
#9689 = DIRECTION ( 'NONE',  ( -0.000000000000000000, 1.000000000000000000, -0.000000000000000000 ) ) ;
#9690 = AXIS2_PLACEMENT_3D ( 'NONE', #19924, #20043, #2633 ) ;
#9691 = AXIS2_PLACEMENT_3D ( 'NONE', #1232, #22442, #14972 ) ;
#9692 = CARTESIAN_POINT ( 'NONE',  ( -8.188149873056859818, 7.413691783916316780, 42.20917188641860918 ) ) ;
#9693 = DIRECTION ( 'NONE',  ( -6.505213034913038160E-19, -3.903127820947822896E-18, -1.000000000000000000 ) ) ;
#9694 = EDGE_CURVE ( 'NONE', #21260, #4006, #22251, .T. ) ;
#9695 = VERTEX_POINT ( 'NONE', #17030 ) ;
#9696 = ORIENTED_EDGE ( 'NONE', *, *, #10802, .T. ) ;
#9697 = AXIS2_PLACEMENT_3D ( 'NONE', #5893, #18264, #4178 ) ;
#9698 = ORIENTED_EDGE ( 'NONE', *, *, #7664, .F. ) ;
#9699 = CARTESIAN_POINT ( 'NONE',  ( -22.38366207802769736, 18.39979965017058916, 58.65857802150431155 ) ) ;
#9700 = ADVANCED_FACE ( 'NONE', ( #19102 ), #15183, .T. ) ;
#9701 = LINE ( 'NONE', #21979, #6748 ) ;
#9702 = AXIS2_PLACEMENT_3D ( 'NONE', #12268, #3467, #14195 ) ;
#9703 = B_SPLINE_CURVE_WITH_KNOTS ( 'NONE', 3,
 ( #8093, #20351, #2594, #15049, #983, #7976 ),
 .UNSPECIFIED., .F., .F.,
 ( 4, 2, 4 ),
 ( 1.749076889608653681E-18, 0.005389490931282762097, 0.01077898186256552246 ),
 .UNSPECIFIED. ) ;
#9704 = DIRECTION ( 'NONE',  ( 6.505213034913038160E-19, 3.903127820947822896E-18, 1.000000000000000000 ) ) ;
#9705 = VECTOR ( 'NONE', #2909, 1000.000000000000000 ) ;
#9706 = FACE_OUTER_BOUND ( 'NONE', #21824, .T. ) ;
#9707 = FACE_OUTER_BOUND ( 'NONE', #18282, .T. ) ;
#9708 = CARTESIAN_POINT ( 'NONE',  ( 6.696867368503558448E-15, 40.00000000000000000, 48.73397172404481381 ) ) ;
#9709 = CARTESIAN_POINT ( 'NONE',  ( -9.103081159019573931, 0.03030367950605317509, -53.87333532811887693 ) ) ;
#9710 = CARTESIAN_POINT ( 'NONE',  ( -3.171145143956212387, 39.94219471343448191, -51.05053423814366909 ) ) ;
#9711 = EDGE_CURVE ( 'NONE', #19741, #13092, #11875, .T. ) ;
#9712 = ORIENTED_EDGE ( 'NONE', *, *, #549, .T. ) ;
#9713 = CARTESIAN_POINT ( 'NONE',  ( -9.958219108218488103, 37.43657071496331668, 57.18097912447552034 ) ) ;
#9714 = CARTESIAN_POINT ( 'NONE',  ( 15.97698236194076316, 7.938033795521543645, 59.50430813415452036 ) ) ;
#9715 = CIRCLE ( 'NONE', #4604, 41.00000000000000000 ) ;
#9716 = DIRECTION ( 'NONE',  ( -0.000000000000000000, 1.000000000000000000, -0.000000000000000000 ) ) ;
#9717 = ORIENTED_EDGE ( 'NONE', *, *, #2607, .F. ) ;
#9718 = AXIS2_PLACEMENT_3D ( 'NONE', #16561, #7855, #14714 ) ;
#9719 = ORIENTED_EDGE ( 'NONE', *, *, #3252, .T. ) ;
#9720 = DIRECTION ( 'NONE',  ( -0.000000000000000000, -1.000000000000000000, -0.000000000000000000 ) ) ;
#9721 = FACE_OUTER_BOUND ( 'NONE', #21418, .T. ) ;
#9722 = VECTOR ( 'NONE', #547, 1000.000000000000000 ) ;
#9723 = EDGE_CURVE ( 'NONE', #1767, #17965, #21882, .T. ) ;
#9724 = EDGE_CURVE ( 'NONE', #16, #21800, #13443, .T. ) ;
#9725 = AXIS2_PLACEMENT_3D ( 'NONE', #18305, #2622, #9594 ) ;
#9726 = CYLINDRICAL_SURFACE ( 'NONE', #12222, 15.00000000000000000 ) ;
#9727 = CARTESIAN_POINT ( 'NONE',  ( 6.122947728378624888, 39.99999999999999289, -52.15215614435199143 ) ) ;
#9728 = CIRCLE ( 'NONE', #1324, 8.999999999999998224 ) ;
#9729 = TOROIDAL_SURFACE ( 'NONE', #18880, 34.90673715956759082, 8.750000000000000000 ) ;
#9730 = ORIENTED_EDGE ( 'NONE', *, *, #10283, .F. ) ;
#9731 = CARTESIAN_POINT ( 'NONE',  ( 0.9019812149625040520, 39.99518069238214224, -49.42305015773394672 ) ) ;
#9732 = CIRCLE ( 'NONE', #1326, 19.99999999999999289 ) ;
#9733 = PLANE ( 'NONE',  #15723 ) ;
#9734 = DIRECTION ( 'NONE',  ( 6.505213034913038160E-19, 3.903127820947822896E-18, 1.000000000000000000 ) ) ;
#9735 = EDGE_CURVE ( 'NONE', #5053, #12342, #6143, .T. ) ;
#9736 = CARTESIAN_POINT ( 'NONE',  ( -2.478395369818712446, 39.99999999999999289, 50.25195616245800778 ) ) ;
#9737 = CARTESIAN_POINT ( 'NONE',  ( 10.74988822578072956, 39.17840323699249439, -54.92437902621830403 ) ) ;
#9738 = CYLINDRICAL_SURFACE ( 'NONE', #15541, 2.499999999999998668 ) ;
#9739 = CIRCLE ( 'NONE', #10823, 49.99999999999998579 ) ;
#9740 = CARTESIAN_POINT ( 'NONE',  ( 42.50000000000000711, -12.00000000000000000, -47.50000000000000000 ) ) ;
#9741 = EDGE_CURVE ( 'NONE', #18413, #20053, #18949, .T. ) ;
#9742 = EDGE_LOOP ( 'NONE', ( #17344, #1430, #8082, #11158 ) ) ;
#9743 = DIRECTION ( 'NONE',  ( -1.000000000000000000, 0.000000000000000000, 0.000000000000000000 ) ) ;
#9744 = FACE_BOUND ( 'NONE', #6951, .T. ) ;
#9745 = SURFACE_STYLE_USAGE ( .BOTH. , #10678 ) ;
#9746 = DIRECTION ( 'NONE',  ( -6.505213034913038160E-19, -3.903127820947822896E-18, -1.000000000000000000 ) ) ;
#9747 = CARTESIAN_POINT ( 'NONE',  ( 3.877306978638209416E-14, -25.00000000000000000, -12.00000000000000355 ) ) ;
#9748 = ORIENTED_EDGE ( 'NONE', *, *, #16176, .F. ) ;
#9749 = CARTESIAN_POINT ( 'NONE',  ( 35.00000000000000000, 2.142135623730931471, 4.258610482196280173E-15 ) ) ;
#9750 = AXIS2_PLACEMENT_3D ( 'NONE', #11815, #10207, #10090 ) ;
#9751 = AXIS2_PLACEMENT_3D ( 'NONE', #1119, #21746, #20147 ) ;
#9752 = EDGE_CURVE ( 'NONE', #5947, #19486, #3303, .T. ) ;
#9753 = CIRCLE ( 'NONE', #18487, 19.11328065563152379 ) ;
#9755 = EDGE_CURVE ( 'NONE', #20463, #20208, #18997, .T. ) ;
#9754 = EDGE_LOOP ( 'NONE', ( #6128, #15914, #19210, #388 ) ) ;
#9756 = ORIENTED_EDGE ( 'NONE', *, *, #1783, .T. ) ;
#9757 = DIRECTION ( 'NONE',  ( 1.000000000000000000, 0.000000000000000000, 0.000000000000000000 ) ) ;
#9758 = ORIENTED_EDGE ( 'NONE', *, *, #10991, .F. ) ;
#9759 = CARTESIAN_POINT ( 'NONE',  ( 16.16773315356744334, 31.81208924699234331, -59.56501305110271716 ) ) ;
#9760 = DIRECTION ( 'NONE',  ( 0.000000000000000000, 0.000000000000000000, -1.000000000000000000 ) ) ;
#9761 = DIRECTION ( 'NONE',  ( 0.000000000000000000, 0.000000000000000000, -1.000000000000000000 ) ) ;
#9762 = DIRECTION ( 'NONE',  ( 0.000000000000000000, 0.000000000000000000, -1.000000000000000000 ) ) ;
#9763 = CARTESIAN_POINT ( 'NONE',  ( 4.985660570713311479, 5.844760174181406143, -40.05045397208984070 ) ) ;
#9764 = ORIENTED_EDGE ( 'NONE', *, *, #10743, .T. ) ;
#9765 = FACE_OUTER_BOUND ( 'NONE', #6497, .T. ) ;
#9766 = B_SPLINE_CURVE_WITH_KNOTS ( 'NONE', 3,
 ( #2813, #11735, #13317, #11516 ),
 .UNSPECIFIED., .F., .F.,
 ( 4, 4 ),
 ( 9.715086409671343166E-07, 0.001929643240672210443 ),
 .UNSPECIFIED. ) ;
#9767 = DIRECTION ( 'NONE',  ( 6.505213034913038160E-19, 3.903127820947822896E-18, 1.000000000000000000 ) ) ;
#9768 = ORIENTED_EDGE ( 'NONE', *, *, #12286, .T. ) ;
#9769 = CARTESIAN_POINT ( 'NONE',  ( -9.855264211176375966, 8.670295722316108566, -43.22210574525156801 ) ) ;
#9770 = AXIS2_PLACEMENT_3D ( 'NONE', #11117, #4373, #19737 ) ;
#9771 = CARTESIAN_POINT ( 'NONE',  ( -21.01101238435552077, 12.07760467057786080, -58.34718853222887702 ) ) ;
#9772 = DIRECTION ( 'NONE',  ( -1.000000000000000000, -1.208970125616077665E-17, 0.000000000000000000 ) ) ;
#9773 = ORIENTED_EDGE ( 'NONE', *, *, #2653, .T. ) ;
#9774 = CARTESIAN_POINT ( 'NONE',  ( -25.00000000000000000, -20.00000000000000000, 6.487780019669002523E-15 ) ) ;
#9775 = CARTESIAN_POINT ( 'NONE',  ( 0.7806882667108998586, 39.98538465716379164, -49.65403242876607237 ) ) ;
#9776 = ORIENTED_EDGE ( 'NONE', *, *, #7504, .T. ) ;
#9777 = DIRECTION ( 'NONE',  ( 0.000000000000000000, 0.000000000000000000, -1.000000000000000000 ) ) ;
#9778 = LINE ( 'NONE', #13297, #22085 ) ;
#9779 = CIRCLE ( 'NONE', #6798, 33.99999999999999289 ) ;
#9780 = ORIENTED_EDGE ( 'NONE', *, *, #17960, .F. ) ;
#9781 = CARTESIAN_POINT ( 'NONE',  ( 12.81940492552829980, 35.37234179763579789, 55.76972854553738301 ) ) ;
#9782 = CARTESIAN_POINT ( 'NONE',  ( 42.50000000000000711, -12.00000000000000000, -47.50000000000000000 ) ) ;
#9783 = CARTESIAN_POINT ( 'NONE',  ( 19.80158170751278135, 22.94611027470399023, -60.57464962002911335 ) ) ;
#9784 = AXIS2_PLACEMENT_3D ( 'NONE', #21692, #7259, #17676 ) ;
#9785 = AXIS2_PLACEMENT_3D ( 'NONE', #18074, #5935, #4007 ) ;
#9787 = ADVANCED_FACE ( 'NONE', ( #5016 ), #8553, .T. ) ;
#9786 = ORIENTED_EDGE ( 'NONE', *, *, #11589, .F. ) ;
#9788 = ORIENTED_EDGE ( 'NONE', *, *, #16695, .T. ) ;
#9789 = EDGE_LOOP ( 'NONE', ( #17663, #13406, #8272, #11359 ) ) ;
#9790 = ORIENTED_EDGE ( 'NONE', *, *, #21239, .T. ) ;
#9791 = CARTESIAN_POINT ( 'NONE',  ( 35.00000000000001421, 0.000000000000000000, 1.540743955509788682E-30 ) ) ;
#9792 = DIRECTION ( 'NONE',  ( -0.000000000000000000, -1.000000000000000000, -0.000000000000000000 ) ) ;
#9793 = AXIS2_PLACEMENT_3D ( 'NONE', #2919, #1178, #13534 ) ;
#9794 = EDGE_CURVE ( 'NONE', #14529, #13542, #17479, .T. ) ;
#9795 = VECTOR ( 'NONE', #21921, 1000.000000000000114 ) ;
#9796 = VERTEX_POINT ( 'NONE', #18653 ) ;
#9797 = CARTESIAN_POINT ( 'NONE',  ( 34.00000000000000000, -6.180736333215569367, 0.000000000000000000 ) ) ;
#9798 = CARTESIAN_POINT ( 'NONE',  ( 24.24871130596423185, 14.00000000000009592, -4.999999999999948486 ) ) ;
#9799 = VERTEX_POINT ( 'NONE', #2960 ) ;
#9800 = CARTESIAN_POINT ( 'NONE',  ( 3.000000000000000444, 15.20112712106396913, 8.485281374238567764 ) ) ;
#9801 = AXIS2_PLACEMENT_3D ( 'NONE', #7709, #21344, #5643 ) ;
#9802 = CARTESIAN_POINT ( 'NONE',  ( 13.56354382738800268, 2.142135623730931471, 56.03997097393685323 ) ) ;
#9803 = VERTEX_POINT ( 'NONE', #10265 ) ;
#9804 = DIRECTION ( 'NONE',  ( -6.505213034913038160E-19, -3.903127820947822896E-18, -1.000000000000000000 ) ) ;
#9805 = CARTESIAN_POINT ( 'NONE',  ( 1.572625745558603905, 24.67014512736903242, 8.879522542765043269 ) ) ;
#9806 = DIRECTION ( 'NONE',  ( 0.000000000000000000, 0.000000000000000000, 1.000000000000000000 ) ) ;
#9807 = CIRCLE ( 'NONE', #6515, 31.50000000000000711 ) ;
#9808 = CARTESIAN_POINT ( 'NONE',  ( -0.1620518412016254406, 39.99984822781879501, 48.85971577061582138 ) ) ;
#9809 = EDGE_CURVE ( 'NONE', #19379, #4478, #19330, .T. ) ;
#9810 = FACE_OUTER_BOUND ( 'NONE', #11953, .T. ) ;
#9811 = AXIS2_PLACEMENT_3D ( 'NONE', #7406, #3865, #16340 ) ;
#9812 = ORIENTED_EDGE ( 'NONE', *, *, #13379, .F. ) ;
#9813 = CIRCLE ( 'NONE', #22643, 19.11328065563151668 ) ;
#9814 = AXIS2_PLACEMENT_3D ( 'NONE', #20285, #22004, #6298 ) ;
#9815 = EDGE_LOOP ( 'NONE', ( #20179, #12551, #19829, #365 ) ) ;
#9816 = AXIS2_PLACEMENT_3D ( 'NONE', #19556, #5238, #3859 ) ;
#9817 = CIRCLE ( 'NONE', #4708, 2.524999999999999467 ) ;
#9818 = ORIENTED_EDGE ( 'NONE', *, *, #14065, .F. ) ;
#9819 = CARTESIAN_POINT ( 'NONE',  ( -19.66835476178583164, 23.72826198822068022, 58.05955247658096141 ) ) ;
#9820 = DIRECTION ( 'NONE',  ( 0.000000000000000000, 0.000000000000000000, -1.000000000000000000 ) ) ;
#9821 = CARTESIAN_POINT ( 'NONE',  ( -10.00000000000000000, 1.499999999999997780, -3.000000000000000000 ) ) ;
#9822 = LINE ( 'NONE', #6494, #4453 ) ;
#9823 = FACE_OUTER_BOUND ( 'NONE', #17736, .T. ) ;
#9824 = CIRCLE ( 'NONE', #5804, 2.500000000000008882 ) ;
#9825 = ORIENTED_EDGE ( 'NONE', *, *, #4636, .F. ) ;
#9826 = DIRECTION ( 'NONE',  ( -0.000000000000000000, 1.000000000000000000, -0.000000000000000000 ) ) ;
#9827 = DIRECTION ( 'NONE',  ( -1.000000000000000000, -1.208970125616044077E-17, 0.000000000000000000 ) ) ;
#9828 = DIRECTION ( 'NONE',  ( -1.000000000000000000, 0.000000000000000000, 0.000000000000000000 ) ) ;
#9829 = CARTESIAN_POINT ( 'NONE',  ( -8.234869854316453797, 38.24532177630956653, -54.56732844084849887 ) ) ;
#9830 = CYLINDRICAL_SURFACE ( 'NONE', #15562, 2.499999999999995115 ) ;
#9831 = EDGE_CURVE ( 'NONE', #12985, #15787, #10149, .T. ) ;
#9832 = VECTOR ( 'NONE', #12749, 1000.000000000000227 ) ;
#9833 = EDGE_LOOP ( 'NONE', ( #2963, #14464, #19078, #13299 ) ) ;
#9834 = DIRECTION ( 'NONE',  ( -0.000000000000000000, -1.000000000000000000, -0.000000000000000000 ) ) ;
#9835 = CYLINDRICAL_SURFACE ( 'NONE', #4770, 50.00000000000000000 ) ;
#9836 = CARTESIAN_POINT ( 'NONE',  ( -32.90000000000058833, 28.00000000000000000, -55.00000000000076028 ) ) ;
#9837 = DIRECTION ( 'NONE',  ( 0.000000000000000000, 1.000000000000000000, 0.000000000000000000 ) ) ;
#9838 = CONICAL_SURFACE ( 'NONE', #10553, 18.00000000000000000, 0.7853981633974466137 ) ;
#9839 = EDGE_CURVE ( 'NONE', #21906, #9166, #3528, .T. ) ;
#9840 = VERTEX_POINT ( 'NONE', #22551 ) ;
#9841 = CARTESIAN_POINT ( 'NONE',  ( 34.99999999999980815, 26.00000000000000355, 54.99999999999922551 ) ) ;
#9842 = CARTESIAN_POINT ( 'NONE',  ( 0.000000000000000000, 29.97499999999999787, 3.999999999999998224 ) ) ;
#9843 = CARTESIAN_POINT ( 'NONE',  ( -42.49999999999996447, 10.00000000000000000, -45.00000000000000711 ) ) ;
#9844=STYLED_ITEM('',(#22720),#17752);
#9845 = AXIS2_PLACEMENT_3D ( 'NONE', #11927, #5180, #22605 ) ;
#9846 = CARTESIAN_POINT ( 'NONE',  ( -0.7280394207210799662, -4.626139448366399343, 46.02403719818684635 ) ) ;
#9847 = EDGE_CURVE ( 'NONE', #13884, #5071, #15261, .T. ) ;
#9848 = DIRECTION ( 'NONE',  ( 6.505213034913038160E-19, 3.903127820947822896E-18, 1.000000000000000000 ) ) ;
#9849 = AXIS2_PLACEMENT_3D ( 'NONE', #15116, #13057, #18583 ) ;
#9850 = ORIENTED_EDGE ( 'NONE', *, *, #9185, .F. ) ;
#9851 = CARTESIAN_POINT ( 'NONE',  ( 10.34137811700566090, 39.99999999999998579, 53.75702834151141474 ) ) ;
#9852 = DIRECTION ( 'NONE',  ( -0.4124789556921616973, 0.7071067811865355823, -0.5743353646704342230 ) ) ;
#9853 = CARTESIAN_POINT ( 'NONE',  ( -34.99999999999999289, 4.000000000000028422, 9.999999999999971578 ) ) ;
#9854 = ADVANCED_FACE ( 'NONE', ( #20589 ), #17145, .F. ) ;
#9855 = CARTESIAN_POINT ( 'NONE',  ( 9.886810796748164876, 39.30595911735670001, -54.61697552245239962 ) ) ;
#9856 = DIRECTION ( 'NONE',  ( -6.505213034913038160E-19, -3.903127820947822896E-18, -1.000000000000000000 ) ) ;
#9857 = CARTESIAN_POINT ( 'NONE',  ( 35.00000000000001421, 0.000000000000000000, -11.00000000000003730 ) ) ;
#9858 = ORIENTED_EDGE ( 'NONE', *, *, #908, .F. ) ;
#9859 = CYLINDRICAL_SURFACE ( 'NONE', #15227, 0.9999999999999974465 ) ;
#9860 = CARTESIAN_POINT ( 'NONE',  ( 5.833333333333336590, 40.00000000000000000, 40.61164310337068173 ) ) ;
#9861 = CARTESIAN_POINT ( 'NONE',  ( -22.26748298433245310, 22.28024240313483517, -2.999999999999975131 ) ) ;
#9862 = CARTESIAN_POINT ( 'NONE',  ( 42.50000000000000711, -12.00000000000000000, -47.50000000000000000 ) ) ;
#9863 = ORIENTED_EDGE ( 'NONE', *, *, #1400, .T. ) ;
#9864 = FACE_OUTER_BOUND ( 'NONE', #11776, .T. ) ;
#9865 = DIRECTION ( 'NONE',  ( 0.000000000000000000, -1.000000000000000000, 0.000000000000000000 ) ) ;
#9866 = ORIENTED_EDGE ( 'NONE', *, *, #9218, .T. ) ;
#9867 = EDGE_CURVE ( 'NONE', #15736, #18333, #19673, .T. ) ;
#9868 = ORIENTED_EDGE ( 'NONE', *, *, #5949, .F. ) ;
#9869 =( LENGTH_UNIT ( ) NAMED_UNIT ( * ) SI_UNIT ( .MILLI., .METRE. ) );
#9870 = ORIENTED_EDGE ( 'NONE', *, *, #10957, .F. ) ;
#9871 = CARTESIAN_POINT ( 'NONE',  ( 16.44544766657915957, 31.39195386311723723, 59.65016313815161197 ) ) ;
#9872 = CARTESIAN_POINT ( 'NONE',  ( -31.57187188083515750, -7.711478842616581453, -7.000000000000006217 ) ) ;
#9873 = LINE ( 'NONE', #16750, #21255 ) ;
#9874 = CARTESIAN_POINT ( 'NONE',  ( 19.23800698326013148, 14.47374112874265073, 60.43633296823762890 ) ) ;
#9875 = ORIENTED_EDGE ( 'NONE', *, *, #21441, .F. ) ;
#9876 = CARTESIAN_POINT ( 'NONE',  ( -34.99999999999999289, -5.000000000000000000, -57.49999999999705125 ) ) ;
#9877 = DIRECTION ( 'NONE',  ( -0.7071067811865524577, 0.000000000000000000, -0.7071067811865426878 ) ) ;
#9878 = ORIENTED_EDGE ( 'NONE', *, *, #921, .T. ) ;
#9879 = EDGE_CURVE ( 'NONE', #14723, #19899, #3972, .T. ) ;
#9880 = DIRECTION ( 'NONE',  ( 1.049727191138617217E-16, 0.5150380749100562650, -0.8571673007021111124 ) ) ;
#9881 = CARTESIAN_POINT ( 'NONE',  ( -87.90000000000000568, 28.00000000000000000, -9.108981535246192915E-16 ) ) ;
#9883 = AXIS2_PLACEMENT_3D ( 'NONE', #449, #17757, #12371 ) ;
#9882 = DIRECTION ( 'NONE',  ( 1.266830946243004623E-16, -1.000000000000000000, -3.903127820947817503E-18 ) ) ;
#9884 = DIRECTION ( 'NONE',  ( 0.000000000000000000, 1.000000000000000000, 0.000000000000000000 ) ) ;
#9885 = EDGE_LOOP ( 'NONE', ( #338, #12360 ) ) ;
#9886 = DIRECTION ( 'NONE',  ( -0.000000000000000000, -0.000000000000000000, 1.000000000000000000 ) ) ;
#9887 = CYLINDRICAL_SURFACE ( 'NONE', #3631, 59.99999999999703704 ) ;
#9888 = VERTEX_POINT ( 'NONE', #10600 ) ;
#9889 = DIRECTION ( 'NONE',  ( 0.000000000000000000, 0.000000000000000000, -1.000000000000000000 ) ) ;
#9890 = CARTESIAN_POINT ( 'NONE',  ( -3.315462071040359060, 0.2472509019876770464, -51.08206760068764396 ) ) ;
#9891 = ORIENTED_EDGE ( 'NONE', *, *, #4382, .F. ) ;
#9892 = CYLINDRICAL_SURFACE ( 'NONE', #5409, 2.499999999999996891 ) ;
#9893 = AXIS2_PLACEMENT_3D ( 'NONE', #11022, #7590, #14788 ) ;
#9894 = DIRECTION ( 'NONE',  ( -0.000000000000000000, -1.000000000000000000, -0.000000000000000000 ) ) ;
#9895 = EDGE_CURVE ( 'NONE', #7376, #20269, #6889, .T. ) ;
#9896 = DIRECTION ( 'NONE',  ( 0.000000000000000000, 0.000000000000000000, 1.000000000000000000 ) ) ;
#9897 = CARTESIAN_POINT ( 'NONE',  ( 17.29817675750046391, 30.08054145047140082, -57.37022932959450117 ) ) ;
#9898 = ORIENTED_EDGE ( 'NONE', *, *, #3809, .F. ) ;
#9899 = CIRCLE ( 'NONE', #4415, 34.90673715956759082 ) ;
#9900 = ORIENTED_EDGE ( 'NONE', *, *, #2402, .T. ) ;
#9901 = ORIENTED_EDGE ( 'NONE', *, *, #7936, .T. ) ;
#9902 = ORIENTED_EDGE ( 'NONE', *, *, #3987, .T. ) ;
#9903 = CARTESIAN_POINT ( 'NONE',  ( 1.848215538220117304, 24.39449834545646212, 6.812673807617342980 ) ) ;
#9904 = CARTESIAN_POINT ( 'NONE',  ( -5.074925817841774212, 32.10132595304123981, -2.999999999999999112 ) ) ;
#9905 = ORIENTED_EDGE ( 'NONE', *, *, #1206, .F. ) ;
#9906 = CARTESIAN_POINT ( 'NONE',  ( 3.330669073875469621E-13, -1.110223024625156540E-13, -2.999999999999971578 ) ) ;
#9907 = CARTESIAN_POINT ( 'NONE',  ( -1.848215538292884208, 13.60550165460329453, 6.812673807599693099 ) ) ;
#9908 = ORIENTED_EDGE ( 'NONE', *, *, #933, .F. ) ;
#9909 = CARTESIAN_POINT ( 'NONE',  ( 90.00000000000000000, 40.00000000000000711, -9.108981535246192915E-16 ) ) ;
#9910 = ORIENTED_EDGE ( 'NONE', *, *, #19541, .T. ) ;
#9911 = CARTESIAN_POINT ( 'NONE',  ( 5.617773668148541510, 39.81214093377761287, -52.56495119878665889 ) ) ;
#9912 = DIRECTION ( 'NONE',  ( -0.7071067811865426878, 8.659560562354874926E-17, 0.7071067811865524577 ) ) ;
#9913 = LINE ( 'NONE', #16904, #14463 ) ;
#9914 = B_SPLINE_CURVE_WITH_KNOTS ( 'NONE', 3,
 ( #8311, #8200, #15164, #9808, #21969, #6259, #16798, #22186, #866, #22309, #13559, #20571, #21851, #6146, #13788, #17234, #20805, #20918, #19312, #17580, #5219, #1665, #3281, #1438, #17349, #6704, #8870, #22653, #15394, #19198, #8646, #22412, #3504, #18854, #6941, #15623, #3160, #13667, #15839, #18974, #11972, #1888, #13902, #153, #21136, #3388, #7147, #1786, #8767, #10129, #10245, #20684, #10465, #1548, #8425, #15507, #5440 ),
 .UNSPECIFIED., .F., .F.,
 ( 4, 2, 1, 1, 1, 2, 2, 2, 1, 1, 1, 2, 2, 2, 1, 1, 1, 2, 2, 2, 1, 1, 1, 1, 2, 2, 2, 1, 1, 1, 1, 1, 1, 2, 2, 2, 2, 4 ),
 ( 0.0001220703125000000000, 0.01574516296385760489, 0.02355670928953641080, 0.02746248245237637234, 0.02941536903379579279, 0.03039181232450494444, 0.03136825561521409261, 0.04699134826655587682, 0.05480289459222675852, 0.05870866775506264346, 0.06066155433648100226, 0.06163799762719056330, 0.06261444091790013822, 0.09386062622063492955, 0.1094837188720028942, 0.1172952651976868488, 0.1212010383605294644, 0.1231539249419507515, 0.1251068115233720524, 0.1875991821288392758, 0.2188453674315729014, 0.2344684600829397003, 0.2422800064086224336, 0.2461857795714643971, 0.2481386661528859616, 0.2500915527343075540, 0.3750762939453137768, 0.4375686645508168882, 0.4688148498535689712, 0.4844379425049449295, 0.4922494888306329641, 0.4961552619934765374, 0.4981081485748984350, 0.4990845918656087732, 0.5000610351563191669, 0.6250457763672394584, 0.7500305175781598610, 1.000000000000000000 ),
 .UNSPECIFIED. ) ;
#9915 = CARTESIAN_POINT ( 'NONE',  ( -11.49399598612409079, 36.39311532300400387, -57.83624353974209953 ) ) ;
#9916 = ADVANCED_FACE ( 'NONE', ( #12543 ), #14024, .T. ) ;
#9917 = CIRCLE ( 'NONE', #32, 2.099999999999997868 ) ;
#9918 = ADVANCED_FACE ( 'NONE', ( #5681 ), #2137, .F. ) ;
#9919 = CARTESIAN_POINT ( 'NONE',  ( 15.49999999999993783, 42.51666049839543149, 100.0000000000000000 ) ) ;
#9920 = EDGE_CURVE ( 'NONE', #10299, #16687, #7990, .T. ) ;
#9921 = ORIENTED_EDGE ( 'NONE', *, *, #18677, .T. ) ;
#9922 = ORIENTED_EDGE ( 'NONE', *, *, #12807, .T. ) ;
#9923 = ORIENTED_EDGE ( 'NONE', *, *, #20893, .F. ) ;
#9924 = CARTESIAN_POINT ( 'NONE',  ( -21.83670385715168649, 14.52494903932916337, 58.53909266577255011 ) ) ;
#9925 = LINE ( 'NONE', #16691, #6343 ) ;
#9926 = CARTESIAN_POINT ( 'NONE',  ( -18.99836266309359800, 13.69920652258249838, -60.37582729383724711 ) ) ;
#9927 = DIRECTION ( 'NONE',  ( 0.000000000000000000, 0.000000000000000000, -1.000000000000000000 ) ) ;
#9928 = ORIENTED_EDGE ( 'NONE', *, *, #20605, .T. ) ;
#9929 = LINE ( 'NONE', #7451, #14197 ) ;
#9930 = DIRECTION ( 'NONE',  ( -0.000000000000000000, -0.000000000000000000, -1.000000000000000000 ) ) ;
#9931 = DIRECTION ( 'NONE',  ( 6.505213034913038160E-19, 3.903127820947822896E-18, 1.000000000000000000 ) ) ;
#9932 = DIRECTION ( 'NONE',  ( -0.000000000000000000, -1.000000000000000000, -0.000000000000000000 ) ) ;
#9933 = AXIS2_PLACEMENT_3D ( 'NONE', #15940, #16062, #19626 ) ;
#9934 = EDGE_LOOP ( 'NONE', ( #22143, #2233, #6558 ) ) ;
#9935 = DIRECTION ( 'NONE',  ( 6.505213034913038160E-19, 3.903127820947822896E-18, 1.000000000000000000 ) ) ;
#9936 = DIRECTION ( 'NONE',  ( -1.000000000000000000, -1.208970125616063644E-17, 0.000000000000000000 ) ) ;
#9937 = ORIENTED_EDGE ( 'NONE', *, *, #18578, .F. ) ;
#9938 = CARTESIAN_POINT ( 'NONE',  ( 5.249999999999976907, 40.00000000000000000, -41.42387596543809991 ) ) ;
#9939 = CARTESIAN_POINT ( 'NONE',  ( 1.734723475976807094E-14, 20.00000000000000000, 70.71067811865476926 ) ) ;
#9940 = DIRECTION ( 'NONE',  ( 0.000000000000000000, -0.000000000000000000, 1.000000000000000000 ) ) ;
#9941 = ORIENTED_EDGE ( 'NONE', *, *, #11043, .T. ) ;
#9942 = EDGE_CURVE ( 'NONE', #21624, #10917, #12655, .T. ) ;
#9943 = ORIENTED_EDGE ( 'NONE', *, *, #2839, .T. ) ;
#9944 = CARTESIAN_POINT ( 'NONE',  ( -14.29266125237881013, 28.07080038625059260, 2.999999999999995559 ) ) ;
#9945 = AXIS2_PLACEMENT_3D ( 'NONE', #2648, #8245, #6079 ) ;
#9946 = DIRECTION ( 'NONE',  ( -1.000000000000000000, 0.000000000000000000, 0.000000000000000000 ) ) ;
#9947 = ORIENTED_EDGE ( 'NONE', *, *, #3531, .F. ) ;
#9948 = EDGE_CURVE ( 'NONE', #9799, #13942, #410, .T. ) ;
#9949 = CARTESIAN_POINT ( 'NONE',  ( -34.99999999999999289, -5.000000000000000000, -5.000000000000030198 ) ) ;
#9950 = CYLINDRICAL_SURFACE ( 'NONE', #2667, 6.499999999999999112 ) ;
#9951 = CARTESIAN_POINT ( 'NONE',  ( -0.7906725175884161683, 39.99999999999998579, 49.24721161524873736 ) ) ;
#9952 = CARTESIAN_POINT ( 'NONE',  ( -21.60080777693147169, 26.06115151610113401, -58.48488838346894880 ) ) ;
#9953 = CARTESIAN_POINT ( 'NONE',  ( -3.022694720415397995, 39.94544410387499056, 50.94009479445880828 ) ) ;
#9954 = DIRECTION ( 'NONE',  ( -0.000000000000000000, -1.000000000000000000, -0.000000000000000000 ) ) ;
#9955 = ORIENTED_EDGE ( 'NONE', *, *, #21210, .F. ) ;
#9956 = CARTESIAN_POINT ( 'NONE',  ( 12.70473862104218732, 28.00863069209355061, 44.75655646380169372 ) ) ;
#9957 = DIRECTION ( 'NONE',  ( -1.000000000000000000, 0.000000000000000000, 0.000000000000000000 ) ) ;
#9958 = CARTESIAN_POINT ( 'NONE',  ( 42.49999999999998579, 10.00000000000000000, -49.99999999999997868 ) ) ;
#9959 = CARTESIAN_POINT ( 'NONE',  ( 35.00000000000001421, 0.000000000000000000, 1.540743955509788682E-30 ) ) ;
#9960 = VECTOR ( 'NONE', #15326, 1000.000000000000000 ) ;
#9961 = ORIENTED_EDGE ( 'NONE', *, *, #18915, .F. ) ;
#9962 = CARTESIAN_POINT ( 'NONE',  ( -35.00000000000000000, 0.000000000000000000, 1.387778780781445676E-14 ) ) ;
#9963 = AXIS2_PLACEMENT_3D ( 'NONE', #14815, #6015, #21839 ) ;
#9964 = DIRECTION ( 'NONE',  ( -1.000000000000000000, 1.764267138144086878E-15, 0.000000000000000000 ) ) ;
#9965 = ADVANCED_FACE ( 'NONE', ( #15986 ), #14258, .F. ) ;
#9966 = EDGE_LOOP ( 'NONE', ( #13352, #2830, #10451, #534 ) ) ;
#9967 = ORIENTED_EDGE ( 'NONE', *, *, #22433, .F. ) ;
#9968 = VERTEX_POINT ( 'NONE', #17941 ) ;
#9969 = FACE_OUTER_BOUND ( 'NONE', #2937, .T. ) ;
#9970 = EDGE_CURVE ( 'NONE', #3873, #13393, #5563, .T. ) ;
#9971 = DIRECTION ( 'NONE',  ( -1.000000000000000000, -1.208970125616063644E-17, 0.000000000000000000 ) ) ;
#9972 = DIRECTION ( 'NONE',  ( -6.505213034913038160E-19, -3.903127820947822896E-18, -1.000000000000000000 ) ) ;
#9973 = DIRECTION ( 'NONE',  ( -0.000000000000000000, 1.000000000000000000, -0.000000000000000000 ) ) ;
#9974 = CARTESIAN_POINT ( 'NONE',  ( -35.00000000000000711, 14.00000000000000000, -38.99999999999997868 ) ) ;
#9975 = ORIENTED_EDGE ( 'NONE', *, *, #21397, .F. ) ;
#9976 = CARTESIAN_POINT ( 'NONE',  ( -34.99999999999980815, 39.97500000000000142, 54.99999999999922551 ) ) ;
#9977 = DIRECTION ( 'NONE',  ( -1.000000000000000000, 0.000000000000000000, 0.000000000000000000 ) ) ;
#9978 = VERTEX_POINT ( 'NONE', #14374 ) ;
#9979 = CARTESIAN_POINT ( 'NONE',  ( -6.426802710256914075, 6.431242889908570071, -41.03786381671499583 ) ) ;
#9980 = CONICAL_SURFACE ( 'NONE', #7416, 59.99999999999700862, 0.7853981633974380649 ) ;
#9981 = CARTESIAN_POINT ( 'NONE',  ( 1.485717122675836999, -1.299971956346730906, -49.29290837556843030 ) ) ;
#9982 = DIRECTION ( 'NONE',  ( 0.000000000000000000, 0.000000000000000000, 1.000000000000000000 ) ) ;
#9983 = CARTESIAN_POINT ( 'NONE',  ( 6.490531240979301231, 40.00000000000000711, 52.32367557809152459 ) ) ;
#9984 = ORIENTED_EDGE ( 'NONE', *, *, #8177, .T. ) ;
#9985 = CARTESIAN_POINT ( 'NONE',  ( 35.00000000000001421, 5.000000000000000000, -9.000000000000035527 ) ) ;
#9986 = VERTEX_POINT ( 'NONE', #13921 ) ;
#9987 = DIRECTION ( 'NONE',  ( -0.000000000000000000, -1.000000000000000000, -0.000000000000000000 ) ) ;
#9988 =( NAMED_UNIT ( * ) PLANE_ANGLE_UNIT ( ) SI_UNIT ( $, .RADIAN. ) );
#9989 = ORIENTED_EDGE ( 'NONE', *, *, #11233, .T. ) ;
#9990 = CARTESIAN_POINT ( 'NONE',  ( -42.50000000000000711, -12.00000000000012434, 50.02500000000011937 ) ) ;
#9991 = EDGE_CURVE ( 'NONE', #2304, #13173, #15659, .T. ) ;
#9992 = CARTESIAN_POINT ( 'NONE',  ( 2.602085213965210642E-15, 0.6398376396478597794, 17.00000000000000711 ) ) ;
#9993 = CARTESIAN_POINT ( 'NONE',  ( 7.310544252644470693E-15, 28.19616000222403684, 0.000000000000000000 ) ) ;
#9994 = CARTESIAN_POINT ( 'NONE',  ( 22.04638094649235569, 24.21359277922482534, -58.58544938243624500 ) ) ;
#9995 = VECTOR ( 'NONE', #21669, 1000.000000000000000 ) ;
#9996 = EDGE_CURVE ( 'NONE', #7279, #10478, #5794, .T. ) ;
#9997 = AXIS2_PLACEMENT_3D ( 'NONE', #16395, #2307, #9300 ) ;
#9998 = ORIENTED_EDGE ( 'NONE', *, *, #5167, .F. ) ;
#9999 = VERTEX_POINT ( 'NONE', #17828 ) ;
#10000 = EDGE_LOOP ( 'NONE', ( #6520, #16161, #750, #4528 ) ) ;
#10001 = DIRECTION ( 'NONE',  ( 1.000000000000000000, -1.296372316667914327E-16, 0.000000000000000000 ) ) ;
#10002 = EDGE_LOOP ( 'NONE', ( #6873, #11731, #19612, #310 ) ) ;
#10003 = DIRECTION ( 'NONE',  ( 6.505213034913038160E-19, 3.903127820947822896E-18, 1.000000000000000000 ) ) ;
#10004 = DIRECTION ( 'NONE',  ( 0.000000000000000000, 0.000000000000000000, -1.000000000000000000 ) ) ;
#10005 = CIRCLE ( 'NONE', #16602, 2.499999999999996891 ) ;
#10006 = EDGE_CURVE ( 'NONE', #626, #5224, #1384, .T. ) ;
#10007 = ORIENTED_EDGE ( 'NONE', *, *, #17772, .F. ) ;
#10008 = DIRECTION ( 'NONE',  ( -6.505213034913038160E-19, -3.903127820947822896E-18, -1.000000000000000000 ) ) ;
#10009 = CARTESIAN_POINT ( 'NONE',  ( -10.27431133777640149, -4.928932188134504955, 51.43682631505699732 ) ) ;
#10010 = EDGE_LOOP ( 'NONE', ( #4731, #22639, #19473, #1134 ) ) ;
#10011 = CARTESIAN_POINT ( 'NONE',  ( 36.06598984771573413, 7.000000000000000000, 48.42385786802029912 ) ) ;
#10012 = CIRCLE ( 'NONE', #16958, 19.11328065563151668 ) ;
#10013 = VERTEX_POINT ( 'NONE', #19220 ) ;
#10014 = DIRECTION ( 'NONE',  ( 1.000000000000000000, 0.000000000000000000, 0.000000000000000000 ) ) ;
#10015 = AXIS2_PLACEMENT_3D ( 'NONE', #18418, #2737, #6054 ) ;
#10016 = EDGE_CURVE ( 'NONE', #4461, #15060, #22649, .T. ) ;
#10017 = DIRECTION ( 'NONE',  ( -1.000000000000000000, -1.208970125616044077E-17, 0.000000000000000000 ) ) ;
#10018 = CARTESIAN_POINT ( 'NONE',  ( -36.14481870267515262, 0.8626474017860440435, 2.932969818539048479 ) ) ;
#10019 = AXIS2_PLACEMENT_3D ( 'NONE', #10523, #17182, #22590 ) ;
#10020 = EDGE_CURVE ( 'NONE', #3259, #7904, #9125, .T. ) ;
#10021 = CARTESIAN_POINT ( 'NONE',  ( -14.04383866228955924, 14.71638174774083119, 45.39674436955353087 ) ) ;
#10022 = ORIENTED_EDGE ( 'NONE', *, *, #4962, .F. ) ;
#10023 = VECTOR ( 'NONE', #7555, 1000.000000000000000 ) ;
#10024 = ORIENTED_EDGE ( 'NONE', *, *, #1245, .T. ) ;
#10025 = ORIENTED_EDGE ( 'NONE', *, *, #20702, .T. ) ;
#10026 = EDGE_CURVE ( 'NONE', #10462, #19879, #15762, .T. ) ;
#10027 = VERTEX_POINT ( 'NONE', #21046 ) ;
#10028 = CARTESIAN_POINT ( 'NONE',  ( -19.45266119884174216, 15.02268094489439854, 60.49039575452388107 ) ) ;
#10029 = CARTESIAN_POINT ( 'NONE',  ( -34.99999999999999289, 1.000000000000044187, 9.999999999999971578 ) ) ;
#10030 = DIRECTION ( 'NONE',  ( -1.000000000000000000, 0.000000000000000000, 0.000000000000000000 ) ) ;
#10031 = DIRECTION ( 'NONE',  ( -1.000000000000000000, -1.208970125616060101E-17, 6.505213034913038160E-19 ) ) ;
#10032 = DIRECTION ( 'NONE',  ( 1.000000000000000000, 1.208970125616053321E-17, 0.000000000000000000 ) ) ;
#10033 = ORIENTED_EDGE ( 'NONE', *, *, #9970, .F. ) ;
#10034 = LINE ( 'NONE', #10263, #18992 ) ;
#10035 = CARTESIAN_POINT ( 'NONE',  ( -5.030996294859122919, 39.99999999999999289, -51.62610382703882550 ) ) ;
#10036 = DIRECTION ( 'NONE',  ( 0.000000000000000000, -1.000000000000000000, 0.000000000000000000 ) ) ;
#10037 = DIRECTION ( 'NONE',  ( 1.296372316667914327E-16, 1.000000000000000000, -0.000000000000000000 ) ) ;
#10038 = CIRCLE ( 'NONE', #160, 60.00000000000000000 ) ;
#10039 = VERTEX_POINT ( 'NONE', #19337 ) ;
#10040 = CARTESIAN_POINT ( 'NONE',  ( -11.53082054607096829, 39.05546563713489405, 55.22070542825204598 ) ) ;
#10041 = ORIENTED_EDGE ( 'NONE', *, *, #527, .T. ) ;
#10042 = DIRECTION ( 'NONE',  ( 6.505213034913038160E-19, 3.903127820947822896E-18, 1.000000000000000000 ) ) ;
#10043 = DIRECTION ( 'NONE',  ( -1.000000000000000000, -1.208970125616060717E-17, 0.000000000000000000 ) ) ;
#10044 = CARTESIAN_POINT ( 'NONE',  ( -9.377138775076113930, -4.928932188134509396, -51.00555535510811467 ) ) ;
#10045 = DIRECTION ( 'NONE',  ( 0.000000000000000000, 1.000000000000000000, 0.000000000000000000 ) ) ;
#10046 = ORIENTED_EDGE ( 'NONE', *, *, #17266, .F. ) ;
#10047 = EDGE_CURVE ( 'NONE', #8764, #13828, #18217, .T. ) ;
#10048 = VERTEX_POINT ( 'NONE', #16560 ) ;
#10049 = VECTOR ( 'NONE', #20990, 1000.000000000000000 ) ;
#10050 = CARTESIAN_POINT ( 'NONE',  ( 35.00000000000000000, 17.00000000000000000, 2.365113165210053967E-14 ) ) ;
#10051 = DIRECTION ( 'NONE',  ( 1.000000000000000000, 0.000000000000000000, 0.000000000000000000 ) ) ;
#10052 = ORIENTED_EDGE ( 'NONE', *, *, #20864, .T. ) ;
#10053 = CARTESIAN_POINT ( 'NONE',  ( 7.033428926742908871, 6.687309450572921143, 41.47353357286038289 ) ) ;
#10054 = EDGE_CURVE ( 'NONE', #8568, #14085, #18509, .T. ) ;
#10055 = CARTESIAN_POINT ( 'NONE',  ( -42.50000000000000711, -12.00000000000000000, 47.50000000000000711 ) ) ;
#10056 = DIRECTION ( 'NONE',  ( 0.000000000000000000, -1.000000000000000000, 0.000000000000000000 ) ) ;
#10057 = CONICAL_SURFACE ( 'NONE', #1663, 22.12933039895921539, 1.308996938995746095 ) ;
#10058 = CARTESIAN_POINT ( 'NONE',  ( -21.32169069720652033, 26.98977702688068092, -58.42023943869688196 ) ) ;
#10059 = DIRECTION ( 'NONE',  ( 6.505213034913038160E-19, 3.903127820947822896E-18, 1.000000000000000000 ) ) ;
#10060 = VECTOR ( 'NONE', #3581, 1000.000000000000000 ) ;
#10061 = CARTESIAN_POINT ( 'NONE',  ( -9.998533603140343118, 40.00000000000000000, 54.54288842742653287 ) ) ;
#10062 = ORIENTED_EDGE ( 'NONE', *, *, #2433, .F. ) ;
#10063 = CARTESIAN_POINT ( 'NONE',  ( 8.759110511859017123, 32.19698383752734827, 42.56552456877081170 ) ) ;
#10064 = LINE ( 'NONE', #3334, #518 ) ;
#10065 = CARTESIAN_POINT ( 'NONE',  ( 11.68987541777365458, 3.735186999670053964, -55.40064774139467119 ) ) ;
#10066 = DIRECTION ( 'NONE',  ( -1.000000000000000000, 0.000000000000000000, 0.000000000000000000 ) ) ;
#10067 = CIRCLE ( 'NONE', #13367, 8.750000000000000000 ) ;
#10068 = VERTEX_POINT ( 'NONE', #18048 ) ;
#10069 = LINE ( 'NONE', #17066, #2121 ) ;
#10070 = DIRECTION ( 'NONE',  ( 1.000000000000000000, 0.000000000000000000, 0.000000000000000000 ) ) ;
#10071 = CARTESIAN_POINT ( 'NONE',  ( 24.73600648735135721, -27.19760187735878532, 2.800654218530481465 ) ) ;
#10072 = DIRECTION ( 'NONE',  ( -6.505213034913038160E-19, -3.903127820947822896E-18, -1.000000000000000000 ) ) ;
#10073 = EDGE_CURVE ( 'NONE', #18457, #8634, #669, .T. ) ;
#10074 = VECTOR ( 'NONE', #1755, 1000.000000000000114 ) ;
#10075 = EDGE_LOOP ( 'NONE', ( #7615, #15556 ) ) ;
#10076 = CIRCLE ( 'NONE', #20348, 2.500000000000008882 ) ;
#10077 = ORIENTED_EDGE ( 'NONE', *, *, #12013, .T. ) ;
#10078 = ORIENTED_EDGE ( 'NONE', *, *, #17016, .T. ) ;
#10079 = DIRECTION ( 'NONE',  ( -0.000000000000000000, 1.000000000000000000, -0.000000000000000000 ) ) ;
#10080 = CIRCLE ( 'NONE', #11921, 0.9999999999999974465 ) ;
#10081 = CARTESIAN_POINT ( 'NONE',  ( 10.39230484541308819, -25.00000000000000000, 6.000000000000008882 ) ) ;
#10082 = DIRECTION ( 'NONE',  ( 0.000000000000000000, -1.000000000000000000, 0.000000000000000000 ) ) ;
#10083 = DIRECTION ( 'NONE',  ( 1.000000000000000000, 0.000000000000000000, -1.445602896647339410E-16 ) ) ;
#10084 = FACE_BOUND ( 'NONE', #398, .T. ) ;
#10085 = ORIENTED_EDGE ( 'NONE', *, *, #5776, .F. ) ;
#10086 = CARTESIAN_POINT ( 'NONE',  ( -17.00000000000002842, 20.00000000000000355, -102.0000000000000142 ) ) ;
#10087 = DIRECTION ( 'NONE',  ( 0.000000000000000000, 0.000000000000000000, -1.000000000000000000 ) ) ;
#10088 = EDGE_LOOP ( 'NONE', ( #1111, #5226, #19794, #857 ) ) ;
#10089 = LINE ( 'NONE', #22490, #1355 ) ;
#10090 = DIRECTION ( 'NONE',  ( 1.000000000000000000, 0.000000000000000000, 0.000000000000000000 ) ) ;
#10091 = CARTESIAN_POINT ( 'NONE',  ( 7.325260514639500961E-15, -4.648749848371387827, 45.43309249825157536 ) ) ;
#10092 = CARTESIAN_POINT ( 'NONE',  ( 35.00000000000000000, -15.00000000000000000, -14.99999999999997691 ) ) ;
#10093 = VERTEX_POINT ( 'NONE', #13215 ) ;
#10094 = CARTESIAN_POINT ( 'NONE',  ( 14.98515767422208000, 20.77155976913489610, -45.81928800960650960 ) ) ;
#10095 = EDGE_LOOP ( 'NONE', ( #9123, #18658, #7528, #12423, #22493, #18080, #2098 ) ) ;
#10096 = CARTESIAN_POINT ( 'NONE',  ( 3.608224830031758756E-13, -2.775557561562891351E-14, -4.999999999999997335 ) ) ;
#10097 = AXIS2_PLACEMENT_3D ( 'NONE', #8058, #948, #21586 ) ;
#10098 = CIRCLE ( 'NONE', #21085, 59.99999999999703704 ) ;
#10099 = CARTESIAN_POINT ( 'NONE',  ( -17.25453130113931621, 34.47978402352275396, 57.33123263757909882 ) ) ;
#10100 = CIRCLE ( 'NONE', #2432, 8.750000000000000000 ) ;
#10101 = ADVANCED_FACE ( 'NONE', ( #4320 ), #9472, .F. ) ;
#10102 = AXIS2_PLACEMENT_3D ( 'NONE', #5163, #330, #17629 ) ;
#10103 = ORIENTED_EDGE ( 'NONE', *, *, #622, .F. ) ;
#10104 = DIRECTION ( 'NONE',  ( 0.1421319796954317316, 0.000000000000000000, -0.9898477157360406897 ) ) ;
#10105 = CARTESIAN_POINT ( 'NONE',  ( 1.734723475976807094E-14, 20.00000000000000000, -70.71067811865476926 ) ) ;
#10106 = CARTESIAN_POINT ( 'NONE',  ( 34.99999999999980815, 26.00000000000000355, 52.89999999999922409 ) ) ;
#10107 = EDGE_CURVE ( 'NONE', #17965, #1767, #17118, .T. ) ;
#10108 = VECTOR ( 'NONE', #21507, 1000.000000000000000 ) ;
#10109 = CARTESIAN_POINT ( 'NONE',  ( 17.11943327291938388, 30.37830191768389199, -59.85657255524078124 ) ) ;
#10110 = ORIENTED_EDGE ( 'NONE', *, *, #20136, .T. ) ;
#10111 = ORIENTED_EDGE ( 'NONE', *, *, #19975, .F. ) ;
#10112 = ORIENTED_EDGE ( 'NONE', *, *, #7753, .T. ) ;
#10113 = VERTEX_POINT ( 'NONE', #20234 ) ;
#10114 = CARTESIAN_POINT ( 'NONE',  ( -42.50000000000000711, -12.00000000000012434, -50.02500000000011227 ) ) ;
#10115 = CARTESIAN_POINT ( 'NONE',  ( -35.00000000000000000, 0.000000000000000000, 39.00000000000002132 ) ) ;
#10116 = FACE_OUTER_BOUND ( 'NONE', #2025, .T. ) ;
#10117 = EDGE_CURVE ( 'NONE', #3077, #9080, #21849, .T. ) ;
#10118 = VERTEX_POINT ( 'NONE', #641 ) ;
#10119 = DIRECTION ( 'NONE',  ( 0.000000000000000000, 0.000000000000000000, 1.000000000000000000 ) ) ;
#10120 = CARTESIAN_POINT ( 'NONE',  ( -3.001573872048556968, -1.099462678412693073, -50.31569927527718988 ) ) ;
#10121 = ORIENTED_EDGE ( 'NONE', *, *, #21039, .F. ) ;
#10122 = AXIS2_PLACEMENT_3D ( 'NONE', #7945, #14906, #6111 ) ;
#10123 = VERTEX_POINT ( 'NONE', #9354 ) ;
#10124 = DIRECTION ( 'NONE',  ( 6.505213034913038160E-19, 3.903127820947822896E-18, 1.000000000000000000 ) ) ;
#10125 = CARTESIAN_POINT ( 'NONE',  ( -10.50000000000012079, 42.51666049839536043, 60.00099999999999767 ) ) ;
#10126 = EDGE_CURVE ( 'NONE', #19594, #7391, #16335, .T. ) ;
#10127 = CARTESIAN_POINT ( 'NONE',  ( -35.79662727779865605, 4.171001175319267062, -2.999999999999971578 ) ) ;
#10128 = EDGE_CURVE ( 'NONE', #2957, #22536, #11421, .T. ) ;
#10129 = CARTESIAN_POINT ( 'NONE',  ( -4.592957628191689068, 39.86863559330478779, 51.95971113232090488 ) ) ;
#10130 = CIRCLE ( 'NONE', #13045, 6.499999999999999112 ) ;
#10131 = AXIS2_PLACEMENT_3D ( 'NONE', #10804, #21251, #22435 ) ;
#10132 = CARTESIAN_POINT ( 'NONE',  ( 8.215393105055619927, 1.749144060402857637, -56.08634520686065628 ) ) ;
#10133 = ORIENTED_EDGE ( 'NONE', *, *, #20469, .T. ) ;
#10134 = ORIENTED_EDGE ( 'NONE', *, *, #6109, .T. ) ;
#10135 = ORIENTED_EDGE ( 'NONE', *, *, #3767, .T. ) ;
#10136 = ORIENTED_EDGE ( 'NONE', *, *, #501, .F. ) ;
#10137 = CARTESIAN_POINT ( 'NONE',  ( -34.99999999999997868, -5.000000000000000000, 52.49999999999698730 ) ) ;
#10138 = DIRECTION ( 'NONE',  ( -0.000000000000000000, 1.000000000000000000, -0.000000000000000000 ) ) ;
#10139 = ADVANCED_FACE ( 'NONE', ( #7633 ), #9688, .F. ) ;
#10140 = AXIS2_PLACEMENT_3D ( 'NONE', #15413, #13811, #6500 ) ;
#10141 = CARTESIAN_POINT ( 'NONE',  ( 2.180219338269464124, 39.97139182024317705, -50.35380048836591982 ) ) ;
#10142 = CYLINDRICAL_SURFACE ( 'NONE', #656, 33.99999999999999289 ) ;
#10143 = DIRECTION ( 'NONE',  ( 0.1421319796954317316, 0.000000000000000000, -0.9898477157360405787 ) ) ;
#10144 = AXIS2_PLACEMENT_3D ( 'NONE', #2614, #9587, #16576 ) ;
#10145 = VERTEX_POINT ( 'NONE', #4200 ) ;
#10146 = CARTESIAN_POINT ( 'NONE',  ( -35.16985127952398926, -10.70799354677417980, 2.800654218530485018 ) ) ;
#10147 = CARTESIAN_POINT ( 'NONE',  ( -1.679961165565412751, 40.00000000000000000, -49.78369075542040179 ) ) ;
#10148 = EDGE_CURVE ( 'NONE', #18353, #15997, #16451, .T. ) ;
#10149 = LINE ( 'NONE', #1460, #2482 ) ;
#10150 = ADVANCED_FACE ( 'NONE', ( #11403 ), #14491, .F. ) ;
#10151 = CYLINDRICAL_SURFACE ( 'NONE', #5333, 1.000000000000000888 ) ;
#10152 = EDGE_CURVE ( 'NONE', #5255, #17600, #19786, .T. ) ;
#10153 = ORIENTED_EDGE ( 'NONE', *, *, #9948, .F. ) ;
#10154 = CIRCLE ( 'NONE', #282, 2.524999999999999467 ) ;
#10155 = LINE ( 'NONE', #5022, #16094 ) ;
#10156 = ORIENTED_EDGE ( 'NONE', *, *, #13058, .T. ) ;
#10157 = VECTOR ( 'NONE', #4949, 1000.000000000000000 ) ;
#10158 = LINE ( 'NONE', #11552, #10763 ) ;
#10159 = CYLINDRICAL_SURFACE ( 'NONE', #2369, 4.000000000000000000 ) ;
#10160 = CYLINDRICAL_SURFACE ( 'NONE', #2435, 1.000000000000001776 ) ;
#10161 = EDGE_CURVE ( 'NONE', #4584, #15969, #5913, .T. ) ;
#10162 = AXIS2_PLACEMENT_3D ( 'NONE', #12429, #292, #7288 ) ;
#10163 = VERTEX_POINT ( 'NONE', #20126 ) ;
#10164 = VERTEX_POINT ( 'NONE', #18172 ) ;
#10165 = CARTESIAN_POINT ( 'NONE',  ( -4.859370622531205441, -0.8506459022589687446, 51.48211018323377886 ) ) ;
#10166 = AXIS2_PLACEMENT_3D ( 'NONE', #11824, #3130, #10104 ) ;
#10167 = CYLINDRICAL_SURFACE ( 'NONE', #17467, 19.11328065563152379 ) ;
#10168 = EDGE_LOOP ( 'NONE', ( #3462, #124 ) ) ;
#10169 = AXIS2_PLACEMENT_3D ( 'NONE', #8086, #18731, #14933 ) ;
#10170 = CIRCLE ( 'NONE', #19720, 36.76383501243555685 ) ;
#10171 = CARTESIAN_POINT ( 'NONE',  ( 2.775557561562891351E-14, -2.775557561562891351E-14, 2.999999999999999112 ) ) ;
#10172 = VECTOR ( 'NONE', #1546, 1000.000000000000000 ) ;
#10173 = DIRECTION ( 'NONE',  ( 0.1421319796954322034, 0.000000000000000000, -0.9898477157360405787 ) ) ;
#10174 = DIRECTION ( 'NONE',  ( 0.000000000000000000, 0.000000000000000000, -1.000000000000000000 ) ) ;
#10175 = CARTESIAN_POINT ( 'NONE',  ( -19.96400288702121273, 18.50890182901837022, -60.61328093326559951 ) ) ;
#10176 = AXIS2_PLACEMENT_3D ( 'NONE', #7445, #10995, #572 ) ;
#10177 = CARTESIAN_POINT ( 'NONE',  ( -11.84669267190941078, 29.23061840495883956, -44.31876460048054156 ) ) ;
#10178 = CARTESIAN_POINT ( 'NONE',  ( -15.06903587914754716, 33.17837898604023650, 59.20328215072075295 ) ) ;
#10179 = VERTEX_POINT ( 'NONE', #2483 ) ;
#10180 = FACE_BOUND ( 'NONE', #6700, .T. ) ;
#10181 = DIRECTION ( 'NONE',  ( 0.000000000000000000, 0.000000000000000000, -1.000000000000000000 ) ) ;
#10182 = DIRECTION ( 'NONE',  ( 0.000000000000000000, 1.000000000000000000, 0.000000000000000000 ) ) ;
#10183 = ADVANCED_FACE ( 'NONE', ( #760 ), #12993, .F. ) ;
#10184 = EDGE_LOOP ( 'NONE', ( #13513, #1647, #17636, #16402 ) ) ;
#10185 = EDGE_CURVE ( 'NONE', #938, #12299, #14713, .T. ) ;
#10186 = AXIS2_PLACEMENT_3D ( 'NONE', #19554, #4088, #296 ) ;
#10187 = CARTESIAN_POINT ( 'NONE',  ( -35.00000000000000000, 40.00000000000000000, -58.99999999999992895 ) ) ;
#10188 = DIRECTION ( 'NONE',  ( -0.000000000000000000, 1.000000000000000000, -0.000000000000000000 ) ) ;
#10189 = AXIS2_PLACEMENT_3D ( 'NONE', #9648, #18592, #16639 ) ;
#10190 = CARTESIAN_POINT ( 'NONE',  ( 21.65063509461118230, 12.49999999999984368, -2.999999999999988898 ) ) ;
#10191 = EDGE_CURVE ( 'NONE', #8443, #2570, #14918, .T. ) ;
#10192 =( GEOMETRIC_REPRESENTATION_CONTEXT ( 3 ) GLOBAL_UNCERTAINTY_ASSIGNED_CONTEXT ( ( #11499 ) ) GLOBAL_UNIT_ASSIGNED_CONTEXT ( ( #15604, #22632, #22292 ) ) REPRESENTATION_CONTEXT ( 'NONE', 'WORKASPACE' ) );
#10193 = VERTEX_POINT ( 'NONE', #17119 ) ;
#10194 = APPLICATION_PROTOCOL_DEFINITION ( 'draft international standard', 'automotive_design', 1998, #84 ) ;
#10195 = ORIENTED_EDGE ( 'NONE', *, *, #8128, .T. ) ;
#10196 = CYLINDRICAL_SURFACE ( 'NONE', #1524, 2.499999999999998668 ) ;
#10197 = CARTESIAN_POINT ( 'NONE',  ( 4.026578693517047114, -4.679980696195654488, 48.24134193083390443 ) ) ;
#10198 = DIRECTION ( 'NONE',  ( 6.505213034913038160E-19, 3.903127820947822896E-18, 1.000000000000000000 ) ) ;
#10199 = CARTESIAN_POINT ( 'NONE',  ( -10.70799354677373572, 35.16985127952371215, 2.800654218530492123 ) ) ;
#10200 = AXIS2_PLACEMENT_3D ( 'NONE', #16236, #2268, #428 ) ;
#10201 = CARTESIAN_POINT ( 'NONE',  ( 24.03323817228486448, -20.36304159388385671, -2.999999999999975131 ) ) ;
#10202 = ORIENTED_EDGE ( 'NONE', *, *, #16466, .F. ) ;
#10204 = VECTOR ( 'NONE', #15014, 1000.000000000000000 ) ;
#10203 = CARTESIAN_POINT ( 'NONE',  ( -11.51554440985547956, 40.00000000000000711, -54.14601575511822773 ) ) ;
#10205 = VERTEX_POINT ( 'NONE', #4875 ) ;
#10206 = CARTESIAN_POINT ( 'NONE',  ( 25.34312177887374062, -20.17230487860824439, 2.999999999999995559 ) ) ;
#10207 = DIRECTION ( 'NONE',  ( 6.505213034913038160E-19, 3.903127820947822896E-18, 1.000000000000000000 ) ) ;
#10208 = EDGE_CURVE ( 'NONE', #9032, #3941, #6594, .T. ) ;
#10209 = FACE_BOUND ( 'NONE', #10722, .T. ) ;
#10210 = DIRECTION ( 'NONE',  ( -0.000000000000000000, -1.000000000000000000, -0.000000000000000000 ) ) ;
#10211 = ORIENTED_EDGE ( 'NONE', *, *, #14707, .T. ) ;
#10212 = FACE_OUTER_BOUND ( 'NONE', #13412, .T. ) ;
#10213 = EDGE_LOOP ( 'NONE', ( #6948, #6986, #444, #21547 ) ) ;
#10214 = CYLINDRICAL_SURFACE ( 'NONE', #10473, 28.00000000000000355 ) ;
#10215 = CARTESIAN_POINT ( 'NONE',  ( -22.25047517524403062, 22.91581175091617695, 58.62998360803281628 ) ) ;
#10216 = EDGE_LOOP ( 'NONE', ( #8540, #19843, #16933, #7143 ) ) ;
#10217 = CYLINDRICAL_SURFACE ( 'NONE', #10507, 25.00000000000000711 ) ;
#10218 = B_SPLINE_CURVE_WITH_KNOTS ( 'NONE', 3,
 ( #1388, #13614, #4941, #5174 ),
 .UNSPECIFIED., .F., .F.,
 ( 4, 4 ),
 ( 0.001875451646902801927, 0.003761979286331116300 ),
 .UNSPECIFIED. ) ;
#10219 = DIRECTION ( 'NONE',  ( 0.000000000000000000, 0.000000000000000000, 1.000000000000000000 ) ) ;
#10220 = LINE ( 'NONE', #7019, #11463 ) ;
#10221 = LINE ( 'NONE', #17213, #528 ) ;
#10222 = CIRCLE ( 'NONE', #3294, 43.25806096964028313 ) ;
#10223 = B_SPLINE_CURVE_WITH_KNOTS ( 'NONE', 3,
 ( #6025, #12992, #11291, #18283 ),
 .UNSPECIFIED., .F., .F.,
 ( 4, 4 ),
 ( 9.545285770017924652E-07, 0.001900595205834839339 ),
 .UNSPECIFIED. ) ;
#10224 = ORIENTED_EDGE ( 'NONE', *, *, #2927, .F. ) ;
#10225 = ORIENTED_EDGE ( 'NONE', *, *, #17511, .F. ) ;
#10226 = VERTEX_POINT ( 'NONE', #20353 ) ;
#10227 = EDGE_CURVE ( 'NONE', #10164, #12187, #1041, .T. ) ;
#10228 = ORIENTED_EDGE ( 'NONE', *, *, #14810, .T. ) ;
#10229 = FACE_OUTER_BOUND ( 'NONE', #15701, .T. ) ;
#10230 = DIRECTION ( 'NONE',  ( -0.000000000000000000, -1.000000000000000000, -0.000000000000000000 ) ) ;
#10231 = CARTESIAN_POINT ( 'NONE',  ( 9.064501325224163963, 40.00000000000000711, -53.36141974371220442 ) ) ;
#10232 = ORIENTED_EDGE ( 'NONE', *, *, #9469, .F. ) ;
#10233 = DIRECTION ( 'NONE',  ( -0.000000000000000000, 1.000000000000000000, -0.000000000000000000 ) ) ;
#10234 = CARTESIAN_POINT ( 'NONE',  ( -1.061447036142183720, 5.028531101166970885, 38.77662560222201904 ) ) ;
#10235 = ORIENTED_EDGE ( 'NONE', *, *, #1499, .T. ) ;
#10236 = CARTESIAN_POINT ( 'NONE',  ( -9.103081159019536628, 0.03030367950604325594, 53.87333532811888404 ) ) ;
#10237 = EDGE_CURVE ( 'NONE', #7020, #6550, #20058, .T. ) ;
#10238 = FACE_OUTER_BOUND ( 'NONE', #15263, .T. ) ;
#10239 = AXIS2_PLACEMENT_3D ( 'NONE', #3414, #14264, #12439 ) ;
#10240 = CARTESIAN_POINT ( 'NONE',  ( 42.50000000000000711, -12.00000000000000000, -49.60000000000000142 ) ) ;
#10241 = ORIENTED_EDGE ( 'NONE', *, *, #21539, .F. ) ;
#10242 = LINE ( 'NONE', #17347, #21069 ) ;
#10243 = CARTESIAN_POINT ( 'NONE',  ( 35.00000000000000000, -4.928932188134504955, 4.258610482196280173E-15 ) ) ;
#10244 = DIRECTION ( 'NONE',  ( 0.000000000000000000, 1.000000000000000000, -0.000000000000000000 ) ) ;
#10245 = CARTESIAN_POINT ( 'NONE',  ( -5.178708363027197947, 39.83382011705033676, 52.32443608441192850 ) ) ;
#10246 = DIRECTION ( 'NONE',  ( 0.000000000000000000, -1.000000000000000000, 0.000000000000000000 ) ) ;
#10247 = AXIS2_PLACEMENT_3D ( 'NONE', #1824, #19359, #87 ) ;
#10248 = DIRECTION ( 'NONE',  ( 0.000000000000000000, 0.000000000000000000, 1.000000000000000000 ) ) ;
#10249 = EDGE_CURVE ( 'NONE', #3928, #12420, #3158, .T. ) ;
#10250 = ORIENTED_EDGE ( 'NONE', *, *, #7919, .F. ) ;
#10251 = ORIENTED_EDGE ( 'NONE', *, *, #1618, .F. ) ;
#10252 = ORIENTED_EDGE ( 'NONE', *, *, #2324, .F. ) ;
#10253 = EDGE_CURVE ( 'NONE', #22196, #4403, #13786, .T. ) ;
#10254 = ORIENTED_EDGE ( 'NONE', *, *, #19838, .F. ) ;
#10255 = CARTESIAN_POINT ( 'NONE',  ( -11.68090480754633376, 3.765577839755392286, 57.90797000640143466 ) ) ;
#10256 = LINE ( 'NONE', #7053, #22446 ) ;
#10257 = B_SPLINE_CURVE_WITH_KNOTS ( 'NONE', 3,
 ( #17236, #1551, #10472, #15511 ),
 .UNSPECIFIED., .F., .F.,
 ( 4, 4 ),
 ( 0.001893031756885730620, 0.003808480026564045606 ),
 .UNSPECIFIED. ) ;
#10258 = DIRECTION ( 'NONE',  ( 1.000000000000000000, 1.208970125616062874E-17, 0.000000000000000000 ) ) ;
#10259 = CARTESIAN_POINT ( 'NONE',  ( 32.09841355226000559, -5.093313992686448799, -6.999999999999992006 ) ) ;
#10260 = CARTESIAN_POINT ( 'NONE',  ( 35.00000000000000000, 39.00000000000000711, 4.258610482196280173E-15 ) ) ;
#10261 = EDGE_CURVE ( 'NONE', #11720, #15580, #13453, .T. ) ;
#10262 = VERTEX_POINT ( 'NONE', #13557 ) ;
#10263 = CARTESIAN_POINT ( 'NONE',  ( -4.074925817841801745, 32.10132595304121850, -6.999999999999950262 ) ) ;
#10264 = CARTESIAN_POINT ( 'NONE',  ( -34.99999999999999289, 1.000000000000044187, -10.00000000000003020 ) ) ;
#10265 = CARTESIAN_POINT ( 'NONE',  ( -14.67611967928904271, 31.67162468655987340, 3.000000000000009770 ) ) ;
#10266 = FACE_OUTER_BOUND ( 'NONE', #12981, .T. ) ;
#10267 = CARTESIAN_POINT ( 'NONE',  ( -12.31876324338268525, -30.07487443287973505, 2.999999999999995559 ) ) ;
#10268 = ORIENTED_EDGE ( 'NONE', *, *, #18355, .T. ) ;
#10269 = CARTESIAN_POINT ( 'NONE',  ( -13.28791054760751322, 34.95496542652811200, 58.55506233662532622 ) ) ;
#10270 = ORIENTED_EDGE ( 'NONE', *, *, #5695, .T. ) ;
#10271 = CARTESIAN_POINT ( 'NONE',  ( 5.074925817841801745, -32.10132595304126824, -6.999999999999999112 ) ) ;
#10272 = DIRECTION ( 'NONE',  ( -0.5840452403773163104, -0.8117211080122302969, 0.000000000000000000 ) ) ;
#10273 = EDGE_CURVE ( 'NONE', #3905, #675, #18969, .T. ) ;
#10274 = LINE ( 'NONE', #12007, #2021 ) ;
#10275 = PLANE ( 'NONE',  #3161 ) ;
#10276 = ORIENTED_EDGE ( 'NONE', *, *, #10683, .F. ) ;
#10277 = ADVANCED_FACE ( 'NONE', ( #20569 ), #18634, .T. ) ;
#10278 = ORIENTED_EDGE ( 'NONE', *, *, #11112, .T. ) ;
#10279 = LINE ( 'NONE', #20952, #8930 ) ;
#10280 = CARTESIAN_POINT ( 'NONE',  ( -18.42595423422129741, -0.9047447100419843125, 0.000000000000000000 ) ) ;
#10281 = VERTEX_POINT ( 'NONE', #12386 ) ;
#10282 = DIRECTION ( 'NONE',  ( 0.000000000000000000, 0.000000000000000000, 1.000000000000000000 ) ) ;
#10283 = EDGE_CURVE ( 'NONE', #10917, #9062, #11853, .T. ) ;
#10284 = DIRECTION ( 'NONE',  ( 6.505213034913038160E-19, 3.903127820947822896E-18, 1.000000000000000000 ) ) ;
#10285 = CARTESIAN_POINT ( 'NONE',  ( 9.708269511265326557, -33.52953626616050542, 3.000000000000002665 ) ) ;
#10286 = CARTESIAN_POINT ( 'NONE',  ( -19.94270148199918680, 21.57319560958785232, -58.13234078200304822 ) ) ;
#10287 = DIRECTION ( 'NONE',  ( -0.000000000000000000, 1.000000000000000000, -0.000000000000000000 ) ) ;
#10288 = EDGE_LOOP ( 'NONE', ( #16784, #13826, #4331, #9613 ) ) ;
#10289 = DIRECTION ( 'NONE',  ( 0.000000000000000000, 0.000000000000000000, 1.000000000000000000 ) ) ;
#10290 = FACE_BOUND ( 'NONE', #8462, .T. ) ;
#10291 = EDGE_CURVE ( 'NONE', #12599, #22498, #15291, .T. ) ;
#10292 = DIRECTION ( 'NONE',  ( -1.000000000000000000, -1.208970125616081209E-17, 0.000000000000000000 ) ) ;
#10293 = DIRECTION ( 'NONE',  ( -6.505213034913038160E-19, -3.903127820947822896E-18, -1.000000000000000000 ) ) ;
#10294 = ORIENTED_EDGE ( 'NONE', *, *, #2716, .F. ) ;
#10295 = ADVANCED_FACE ( 'NONE', ( #22184 ), #20075, .F. ) ;
#10296 = DIRECTION ( 'NONE',  ( 0.000000000000000000, 0.000000000000000000, 1.000000000000000000 ) ) ;
#10297 = CARTESIAN_POINT ( 'NONE',  ( 1.010333609296566156E-15, 30.00000000000000000, 7.500000000000000000 ) ) ;
#10298 = AXIS2_PLACEMENT_3D ( 'NONE', #16726, #14874, #1035 ) ;
#10299 = VERTEX_POINT ( 'NONE', #17232 ) ;
#10300 = PRODUCT_CONTEXT ( 'NONE', #12230, 'mechanical' ) ;
#10301 = EDGE_CURVE ( 'NONE', #17346, #6975, #3699, .T. ) ;
#10302 = EDGE_LOOP ( 'NONE', ( #11456, #17918, #5283, #12593 ) ) ;
#10303 = DIRECTION ( 'NONE',  ( 1.000000000000000000, 0.000000000000000000, 0.000000000000000000 ) ) ;
#10304 = CARTESIAN_POINT ( 'NONE',  ( -0.7921581640149152337, 13.00083933660714663, 8.999720221271109821 ) ) ;
#10305 = DIRECTION ( 'NONE',  ( 6.505213034913038160E-19, 3.903127820947822896E-18, 1.000000000000000000 ) ) ;
#10306 = ADVANCED_FACE ( 'NONE', ( #8198 ), #8356, .T. ) ;
#10307 = DIRECTION ( 'NONE',  ( 1.000000000000000000, 0.000000000000000000, 0.000000000000000000 ) ) ;
#10308 = ORIENTED_EDGE ( 'NONE', *, *, #13457, .T. ) ;
#10309 = CARTESIAN_POINT ( 'NONE',  ( 34.99999999999980815, 26.00000000000000355, 57.09999999999921982 ) ) ;
#10310 = CARTESIAN_POINT ( 'NONE',  ( -10.45842016914155259, 40.00000000000001421, -53.79442460303518203 ) ) ;
#10311 = VERTEX_POINT ( 'NONE', #22526 ) ;
#10312 = DIRECTION ( 'NONE',  ( 0.4124789556921606426, 0.7071067811865359154, -0.5743353646704345561 ) ) ;
#10313 = DIRECTION ( 'NONE',  ( 0.000000000000000000, -1.000000000000000000, 0.000000000000000000 ) ) ;
#10314 = CARTESIAN_POINT ( 'NONE',  ( -35.00000000000000000, -5.000000000000000888, 18.00000000000001421 ) ) ;
#10315 = CARTESIAN_POINT ( 'NONE',  ( 0.7351295361033751696, 39.99998559611954363, 49.30628084492604302 ) ) ;
#10316 = CARTESIAN_POINT ( 'NONE',  ( 8.759110511859015347, 32.19698383752734827, -42.56552456877079038 ) ) ;
#10317 = ADVANCED_FACE ( 'NONE', ( #8095 ), #22068, .T. ) ;
#10318 = EDGE_LOOP ( 'NONE', ( #16959, #15403, #18650 ) ) ;
#10319 = CARTESIAN_POINT ( 'NONE',  ( 14.67611967928950101, -31.67162468656004037, -2.999999999999995559 ) ) ;
#10320 = ORIENTED_EDGE ( 'NONE', *, *, #16707, .F. ) ;
#10321 = DIRECTION ( 'NONE',  ( -0.000000000000000000, 1.000000000000000000, -0.000000000000000000 ) ) ;
#10322 = CARTESIAN_POINT ( 'NONE',  ( -42.50000000000000711, -12.00000000000000000, 41.00000000000000711 ) ) ;
#10323 = DIRECTION ( 'NONE',  ( 1.296372316667914327E-16, 1.000000000000000000, -0.000000000000000000 ) ) ;
#10324 = FACE_BOUND ( 'NONE', #8582, .T. ) ;
#10325 = VERTEX_POINT ( 'NONE', #17006 ) ;
#10326 = CIRCLE ( 'NONE', #458, 0.9999999999999974465 ) ;
#10327 = AXIS2_PLACEMENT_3D ( 'NONE', #22634, #1650, #8630 ) ;
#10328 = ORIENTED_EDGE ( 'NONE', *, *, #5558, .T. ) ;
#10329 = ORIENTED_EDGE ( 'NONE', *, *, #9143, .T. ) ;
#10330 = DIRECTION ( 'NONE',  ( 0.000000000000000000, -0.000000000000000000, -1.000000000000000000 ) ) ;
#10331 = VECTOR ( 'NONE', #17466, 1000.000000000000000 ) ;
#10332 = EDGE_CURVE ( 'NONE', #13358, #8824, #8309, .T. ) ;
#10333 = VERTEX_POINT ( 'NONE', #9411 ) ;
#10334 = FACE_BOUND ( 'NONE', #16383, .T. ) ;
#10335 = CARTESIAN_POINT ( 'NONE',  ( 21.01101238435548879, 12.07760467057785370, 58.34718853222888413 ) ) ;
#10336 = CARTESIAN_POINT ( 'NONE',  ( -22.98755168577413954, -22.97438720605751783, 2.999999999999999112 ) ) ;
#10337 = ORIENTED_EDGE ( 'NONE', *, *, #21970, .T. ) ;
#10338 = DIRECTION ( 'NONE',  ( 0.000000000000000000, 0.000000000000000000, -1.000000000000000000 ) ) ;
#10339 = DIRECTION ( 'NONE',  ( -0.000000000000000000, 1.000000000000000000, -0.000000000000000000 ) ) ;
#10340 = ORIENTED_EDGE ( 'NONE', *, *, #19895, .F. ) ;
#10341 = ORIENTED_EDGE ( 'NONE', *, *, #8081, .F. ) ;
#10342 = CARTESIAN_POINT ( 'NONE',  ( -34.99999999999999289, 5.000000000000000000, -3.012171160963566127E-14 ) ) ;
#10343 = ADVANCED_FACE ( 'NONE', ( #705, #16150, #21561, #7687 ), #17995, .T. ) ;
#10344 = ORIENTED_EDGE ( 'NONE', *, *, #3992, .T. ) ;
#10345 = CARTESIAN_POINT ( 'NONE',  ( -2.422192751863949667, -32.40961249803553557, -2.999999999999971578 ) ) ;
#10346 = CARTESIAN_POINT ( 'NONE',  ( -42.49999999999996447, 10.00000000000000000, -54.00000000000000711 ) ) ;
#10347 = CARTESIAN_POINT ( 'NONE',  ( 35.00000000000001421, 5.000000000000000000, -9.000000000000035527 ) ) ;
#10348 = AXIS2_PLACEMENT_3D ( 'NONE', #13801, #1798, #19212 ) ;
#10349 = CARTESIAN_POINT ( 'NONE',  ( 16.49514046905077436, 8.656442121910195908, 59.66722042020315797 ) ) ;
#10350 = CARTESIAN_POINT ( 'NONE',  ( -34.99999999999997868, -5.000000000000000000, 57.49999999999699440 ) ) ;
#10351 = CIRCLE ( 'NONE', #21336, 4.000000000000000000 ) ;
#10352 = AXIS2_PLACEMENT_3D ( 'NONE', #3367, #10323, #1638 ) ;
#10353 = EDGE_CURVE ( 'NONE', #18007, #13854, #7268, .T. ) ;
#10354 = LINE ( 'NONE', #19084, #7822 ) ;
#10355 = ORIENTED_EDGE ( 'NONE', *, *, #20821, .F. ) ;
#10356 = EDGE_CURVE ( 'NONE', #2703, #1700, #4197, .T. ) ;
#10357 = ORIENTED_EDGE ( 'NONE', *, *, #12295, .T. ) ;
#10358 = ORIENTED_EDGE ( 'NONE', *, *, #9179, .F. ) ;
#10359 = ORIENTED_EDGE ( 'NONE', *, *, #16714, .T. ) ;
#10360 = FACE_OUTER_BOUND ( 'NONE', #17131, .T. ) ;
#10361 = CARTESIAN_POINT ( 'NONE',  ( 28.52469787935786982, 10.00000000000000000, -4.095854054471906203 ) ) ;
#10362 = B_SPLINE_SURFACE_WITH_KNOTS ( 'NONE', 1, 3, ( 
 ( #6190, #9851, #16720, #21773, #2410, #9615 ),
 ( #5846, #14649, #21893, #16493, #6070, #13036 ) ),
 .UNSPECIFIED., .F., .F., .F.,
 ( 2, 2 ),
 ( 4, 2, 4 ),
 ( 0.000000000000000000, 1.000000000000000000 ),
 ( 0.000000000000000000, 0.001214050925800256708, 0.002428101851600513415 ),
 .UNSPECIFIED. ) ;
#10363 = AXIS2_PLACEMENT_3D ( 'NONE', #2849, #9834, #13137 ) ;
#10364 = AXIS2_PLACEMENT_3D ( 'NONE', #16618, #926, #16391 ) ;
#10365 = DIRECTION ( 'NONE',  ( 0.000000000000000000, 1.000000000000000000, 0.000000000000000000 ) ) ;
#10366 = CARTESIAN_POINT ( 'NONE',  ( -90.00000000000000000, 26.00000000000000355, -2.099999999999991651 ) ) ;
#10367 = CARTESIAN_POINT ( 'NONE',  ( 2.175252786020501983, 39.97152392022739775, 50.35028940454238011 ) ) ;
#10368 = AXIS2_PLACEMENT_3D ( 'NONE', #2279, #5840, #21081 ) ;
#10369 = ORIENTED_EDGE ( 'NONE', *, *, #2498, .F. ) ;
#10370 = CARTESIAN_POINT ( 'NONE',  ( -33.52953626616031357, -9.708269511265493534, 3.000000000000016431 ) ) ;
#10371 = DIRECTION ( 'NONE',  ( -0.000000000000000000, -1.000000000000000000, -0.000000000000000000 ) ) ;
#10372 = DIRECTION ( 'NONE',  ( 0.000000000000000000, 0.000000000000000000, 1.000000000000000000 ) ) ;
#10373 = DIRECTION ( 'NONE',  ( -0.000000000000000000, -0.000000000000000000, 1.000000000000000000 ) ) ;
#10374 = VERTEX_POINT ( 'NONE', #14315 ) ;
#10375 = CARTESIAN_POINT ( 'NONE',  ( -19.92971843794357056, 21.94076660514457089, 60.60536071356336407 ) ) ;
#10376 = EDGE_CURVE ( 'NONE', #20150, #14303, #20722, .T. ) ;
#10377 = ORIENTED_EDGE ( 'NONE', *, *, #8821, .T. ) ;
#10378 = AXIS2_PLACEMENT_3D ( 'NONE', #5815, #12788, #18061 ) ;
#10379 = CARTESIAN_POINT ( 'NONE',  ( -8.331955809010665348, 38.18181818181817277, 56.36098470834075158 ) ) ;
#10380 = CARTESIAN_POINT ( 'NONE',  ( -35.00000000000000000, 2.142135623730931471, 1.387778780781445676E-14 ) ) ;
#10381 = DIRECTION ( 'NONE',  ( -6.505213034913038160E-19, -3.903127820947822896E-18, -1.000000000000000000 ) ) ;
#10382 = CIRCLE ( 'NONE', #21381, 4.000000000000000000 ) ;
#10383 = ORIENTED_EDGE ( 'NONE', *, *, #18832, .T. ) ;
#10384 = ADVANCED_FACE ( 'NONE', ( #239 ), #15110, .F. ) ;
#10385 = ORIENTED_EDGE ( 'NONE', *, *, #11936, .T. ) ;
#10386 = ORIENTED_EDGE ( 'NONE', *, *, #5057, .F. ) ;
#10387 = CARTESIAN_POINT ( 'NONE',  ( 2.066061548970023143, -1.174227811084479489, -49.70141618117591520 ) ) ;
#10388 = DIRECTION ( 'NONE',  ( 0.000000000000000000, 0.000000000000000000, -1.000000000000000000 ) ) ;
#10389 = VERTEX_POINT ( 'NONE', #9294 ) ;
#10390 = FACE_OUTER_BOUND ( 'NONE', #12639, .T. ) ;
#10391 = ADVANCED_FACE ( 'NONE', ( #2192 ), #10764, .F. ) ;
#10392 = DIRECTION ( 'NONE',  ( -1.000000000000000000, 0.000000000000000000, 0.000000000000000000 ) ) ;
#10393 = DIRECTION ( 'NONE',  ( 0.000000000000000000, -1.000000000000000000, 0.000000000000000000 ) ) ;
#10394 = CARTESIAN_POINT ( 'NONE',  ( -22.38103533145807944, 18.35979201191610244, -58.65801380639353368 ) ) ;
#10395 = CIRCLE ( 'NONE', #12239, 57.00000000000002132 ) ;
#10396 = DIRECTION ( 'NONE',  ( -0.000000000000000000, -1.000000000000000000, -0.000000000000000000 ) ) ;
#10397 = ORIENTED_EDGE ( 'NONE', *, *, #1668, .T. ) ;
#10398 = DIRECTION ( 'NONE',  ( 0.000000000000000000, 0.000000000000000000, 1.000000000000000000 ) ) ;
#10399 = DIRECTION ( 'NONE',  ( -6.505213034913038160E-19, -3.903127820947822896E-18, -1.000000000000000000 ) ) ;
#10400 = DIRECTION ( 'NONE',  ( 0.000000000000000000, 0.000000000000000000, 1.000000000000000000 ) ) ;
#10401 = EDGE_CURVE ( 'NONE', #922, #16909, #12596, .T. ) ;
#10402 = EDGE_CURVE ( 'NONE', #1538, #1187, #14409, .T. ) ;
#10403 = CARTESIAN_POINT ( 'NONE',  ( -31.21605069118050935, -8.646032897229344982, 3.000000000000023537 ) ) ;
#10404 = ORIENTED_EDGE ( 'NONE', *, *, #22691, .T. ) ;
#10405 = AXIS2_PLACEMENT_3D ( 'NONE', #3192, #15079, #3073 ) ;
#10406 = DIRECTION ( 'NONE',  ( -1.000000000000000000, -1.208970125616060717E-17, 0.000000000000000000 ) ) ;
#10407 = FACE_OUTER_BOUND ( 'NONE', #1906, .T. ) ;
#10408 = AXIS2_PLACEMENT_3D ( 'NONE', #12115, #5246, #7181 ) ;
#10409 = ORIENTED_EDGE ( 'NONE', *, *, #16566, .F. ) ;
#10410 = PRODUCT_CONTEXT ( 'NONE', #16917, 'mechanical' ) ;
#10411 = AXIS2_PLACEMENT_3D ( 'NONE', #2392, #4011, #5590 ) ;
#10412 = B_SPLINE_CURVE_WITH_KNOTS ( 'NONE', 3,
 ( #15284, #986, #16677, #2823 ),
 .UNSPECIFIED., .F., .F.,
 ( 4, 4 ),
 ( 9.545285769851497501E-07, 0.001900595205834582383 ),
 .UNSPECIFIED. ) ;
#10413 = VERTEX_POINT ( 'NONE', #2076 ) ;
#10414 = CARTESIAN_POINT ( 'NONE',  ( 42.50000000000000711, -12.00000000000000000, 47.50000000000000711 ) ) ;
#10415 = DIRECTION ( 'NONE',  ( -1.000000000000000000, 1.445602896647339410E-16, 0.000000000000000000 ) ) ;
#10416 = AXIS2_PLACEMENT_3D ( 'NONE', #10759, #12591, #19275 ) ;
#10417 = FACE_OUTER_BOUND ( 'NONE', #3895, .T. ) ;
#10418 = EDGE_CURVE ( 'NONE', #11348, #21191, #18079, .T. ) ;
#10419 = CARTESIAN_POINT ( 'NONE',  ( 11.86180952233169705, 39.00000000000000000, 55.35904751184887118 ) ) ;
#10420 = ORIENTED_EDGE ( 'NONE', *, *, #22366, .F. ) ;
#10421 = CARTESIAN_POINT ( 'NONE',  ( -10.00000000000000000, 1.499999999999997780, -3.000000000000000000 ) ) ;
#10422 = CARTESIAN_POINT ( 'NONE',  ( -9.952189117650851458, 40.00000000000000000, -53.64426396172072486 ) ) ;
#10423 = ORIENTED_EDGE ( 'NONE', *, *, #3335, .F. ) ;
#10424 = CARTESIAN_POINT ( 'NONE',  ( 5.816608766684120191, -4.770324936805535820, -49.23968220743348922 ) ) ;
#10425 = CARTESIAN_POINT ( 'NONE',  ( 13.56354382738798847, 2.142135623730931471, -56.03997097393683191 ) ) ;
#10426 = VECTOR ( 'NONE', #4624, 1000.000000000000000 ) ;
#10427 = DIRECTION ( 'NONE',  ( 0.000000000000000000, 0.000000000000000000, 1.000000000000000000 ) ) ;
#10428 = LINE ( 'NONE', #17426, #1682 ) ;
#10429 = CARTESIAN_POINT ( 'NONE',  ( 14.99999999999998579, 20.00000000000000355, -45.82575694955836809 ) ) ;
#10430 = ORIENTED_EDGE ( 'NONE', *, *, #12491, .T. ) ;
#10431 = DIRECTION ( 'NONE',  ( 1.000000000000000000, 0.000000000000000000, 0.000000000000000000 ) ) ;
#10432 = EDGE_CURVE ( 'NONE', #21559, #11580, #10382, .T. ) ;
#10433 = ADVANCED_FACE ( 'NONE', ( #17890 ), #9177, .T. ) ;
#10434 = CARTESIAN_POINT ( 'NONE',  ( -17.14099744770040701, 5.493236686326245177, 57.28126710884286155 ) ) ;
#10435 = VERTEX_POINT ( 'NONE', #6082 ) ;
#10436 = DIRECTION ( 'NONE',  ( -6.505213034913038160E-19, -3.903127820947822896E-18, -1.000000000000000000 ) ) ;
#10437 = DIRECTION ( 'NONE',  ( -0.000000000000000000, -0.000000000000000000, -1.000000000000000000 ) ) ;
#10438 = AXIS2_PLACEMENT_3D ( 'NONE', #14556, #2306, #14776 ) ;
#10439 = EDGE_CURVE ( 'NONE', #18993, #12370, #13497, .T. ) ;
#10440 = TOROIDAL_SURFACE ( 'NONE', #203, 34.90673715956759082, 8.750000000000000000 ) ;
#10441 = EDGE_CURVE ( 'NONE', #10027, #8509, #19199, .T. ) ;
#10442 = VECTOR ( 'NONE', #21080, 1000.000000000000000 ) ;
#10443 = EDGE_LOOP ( 'NONE', ( #10535, #14136, #783, #18117 ) ) ;
#10444 = TOROIDAL_SURFACE ( 'NONE', #18871, 34.90673715956759082, 8.750000000000000000 ) ;
#10445 = ORIENTED_EDGE ( 'NONE', *, *, #10185, .T. ) ;
#10446 = ORIENTED_EDGE ( 'NONE', *, *, #22691, .F. ) ;
#10447 = ORIENTED_EDGE ( 'NONE', *, *, #20437, .F. ) ;
#10448 = DIRECTION ( 'NONE',  ( 1.776356839400250070E-15, 0.000000000000000000, 1.000000000000000000 ) ) ;
#10449 = CARTESIAN_POINT ( 'NONE',  ( -11.85401191286875111, -32.83234229683740324, 3.000000000000023537 ) ) ;
#10450 = CARTESIAN_POINT ( 'NONE',  ( 9.100109602677072473, 40.00000000000000000, 53.37249912551077102 ) ) ;
#10451 = ORIENTED_EDGE ( 'NONE', *, *, #14354, .T. ) ;
#10452 = LINE ( 'NONE', #1428, #2508 ) ;
#10453 = CARTESIAN_POINT ( 'NONE',  ( -2.859979007343815383, 5.272989970146413796, 39.14811524457574166 ) ) ;
#10454 = ORIENTED_EDGE ( 'NONE', *, *, #14532, .F. ) ;
#10455 = AXIS2_PLACEMENT_3D ( 'NONE', #18527, #487, #10670 ) ;
#10456 = FACE_OUTER_BOUND ( 'NONE', #21467, .T. ) ;
#10457 = AXIS2_PLACEMENT_3D ( 'NONE', #12324, #5350, #17940 ) ;
#10458 = CARTESIAN_POINT ( 'NONE',  ( 6.889846921705527817E-15, -1.896945173645837590, 47.89158637319812328 ) ) ;
#10459 = AXIS2_PLACEMENT_3D ( 'NONE', #20741, #7201, #19024 ) ;
#10460 = ORIENTED_EDGE ( 'NONE', *, *, #9212, .F. ) ;
#10461 = CARTESIAN_POINT ( 'NONE',  ( 2.859979007343827817, 34.72701002985358087, 39.14811524457574876 ) ) ;
#10462 = VERTEX_POINT ( 'NONE', #18448 ) ;
#10463 = DIRECTION ( 'NONE',  ( 0.000000000000000000, 0.000000000000000000, 1.000000000000000000 ) ) ;
#10464 = CYLINDRICAL_SURFACE ( 'NONE', #15569, 36.76383501243555685 ) ;
#10465 = CARTESIAN_POINT ( 'NONE',  ( -6.745305152897880241, 39.70676899211738942, 53.21562672405194405 ) ) ;
#10466 = CONICAL_SURFACE ( 'NONE', #6461, 49.99999999999998579, 0.7853981633974691512 ) ;
#10467 = PLANE ( 'NONE',  #6037 ) ;
#10468 = CARTESIAN_POINT ( 'NONE',  ( 24.79619811426203668, -21.00948735876886886, -2.999999999999999112 ) ) ;
#10469 = EDGE_CURVE ( 'NONE', #7786, #2949, #6023, .T. ) ;
#10470 = DIRECTION ( 'NONE',  ( 0.000000000000000000, -1.000000000000000000, 0.000000000000000000 ) ) ;
#10471 = EDGE_CURVE ( 'NONE', #8574, #9695, #3455, .T. ) ;
#10472 = CARTESIAN_POINT ( 'NONE',  ( 10.35112103033899622, -34.64554704988861999, -2.932164912090521991 ) ) ;
#10473 = AXIS2_PLACEMENT_3D ( 'NONE', #10096, #15135, #6336 ) ;
#10474 = ORIENTED_EDGE ( 'NONE', *, *, #8194, .T. ) ;
#10475 = ORIENTED_EDGE ( 'NONE', *, *, #13576, .F. ) ;
#10476 = ADVANCED_FACE ( 'NONE', ( #16948 ), #14780, .T. ) ;
#10477 = VERTEX_POINT ( 'NONE', #4374 ) ;
#10478 = VERTEX_POINT ( 'NONE', #9626 ) ;
#10479 = CARTESIAN_POINT ( 'NONE',  ( -15.00671337312635067, 3.288799316214447988, 56.57538198732753898 ) ) ;
#10480 = DIRECTION ( 'NONE',  ( -6.505213034913038160E-19, -3.903127820947822896E-18, -1.000000000000000000 ) ) ;
#10481 = CARTESIAN_POINT ( 'NONE',  ( -8.485281374238345720, -3.000000000000002665, 4.999999999999993783 ) ) ;
#10482 = CARTESIAN_POINT ( 'NONE',  ( -35.00000000000000000, 39.00000000000000711, -49.99999999999997158 ) ) ;
#10483 = CARTESIAN_POINT ( 'NONE',  ( 0.08083351145619603606, 39.99996233019618330, 48.79679892491352433 ) ) ;
#10484 = ORIENTED_EDGE ( 'NONE', *, *, #10697, .T. ) ;
#10485 = DIRECTION ( 'NONE',  ( 0.000000000000000000, 0.000000000000000000, -1.000000000000000000 ) ) ;
#10486 = CYLINDRICAL_SURFACE ( 'NONE', #19258, 2.500000000000002220 ) ;
#10487 = DIRECTION ( 'NONE',  ( 0.000000000000000000, 0.000000000000000000, 1.000000000000000000 ) ) ;
#10488 = DIRECTION ( 'NONE',  ( -6.505213034913038160E-19, -3.903127820947822896E-18, -1.000000000000000000 ) ) ;
#10489 = CONICAL_SURFACE ( 'NONE', #624, 9.000000000000035527, 0.7853981633974447263 ) ;
#10490 = DIRECTION ( 'NONE',  ( -1.000000000000000000, 0.000000000000000000, 0.000000000000000000 ) ) ;
#10491 = ADVANCED_FACE ( 'NONE', ( #16617 ), #925, .F. ) ;
#10492 = ORIENTED_EDGE ( 'NONE', *, *, #22039, .T. ) ;
#10493 = CYLINDRICAL_SURFACE ( 'NONE', #5058, 0.9999999999999974465 ) ;
#10494 = CARTESIAN_POINT ( 'NONE',  ( -7.938322399564284204, 38.36220367130332676, 56.16250688144528169 ) ) ;
#10495 = DIRECTION ( 'NONE',  ( -0.000000000000000000, 1.000000000000000000, -0.000000000000000000 ) ) ;
#10496 = DIRECTION ( 'NONE',  ( 1.000000000000000000, 1.208970125616063028E-17, 0.000000000000000000 ) ) ;
#10497 = EDGE_LOOP ( 'NONE', ( #18057, #4027, #4048 ) ) ;
#10498 = EDGE_LOOP ( 'NONE', ( #15334, #9051, #7592, #22448 ) ) ;
#10499 = CIRCLE ( 'NONE', #3198, 3.999999999999994671 ) ;
#10500 = CIRCLE ( 'NONE', #4674, 34.90673715956759082 ) ;
#10501 = EDGE_LOOP ( 'NONE', ( #2649, #15089, #22393 ) ) ;
#10502 = CARTESIAN_POINT ( 'NONE',  ( -0.05567163769003378310, -4.650449146058907246, -45.38800358221576658 ) ) ;
#10503 = CARTESIAN_POINT ( 'NONE',  ( -32.28023859650863159, -14.85562396683518749, -2.999999999999995559 ) ) ;
#10504 = ORIENTED_EDGE ( 'NONE', *, *, #16466, .T. ) ;
#10505 = EDGE_CURVE ( 'NONE', #17804, #14924, #3089, .T. ) ;
#10506 = PRODUCT_DEFINITION ( 'UNKNOWN', '', #9115, #16210 ) ;
#10507 = AXIS2_PLACEMENT_3D ( 'NONE', #15372, #8174, #1523 ) ;
#10508 = CARTESIAN_POINT ( 'NONE',  ( 15.99999999999991651, 20.00000000000000000, 102.0000000000000142 ) ) ;
#10509 = DIRECTION ( 'NONE',  ( 0.000000000000000000, 0.000000000000000000, -1.000000000000000000 ) ) ;
#10510 = CARTESIAN_POINT ( 'NONE',  ( -12.50843255120859965, 35.62740313860118135, -55.64392373821144133 ) ) ;
#10511 = CARTESIAN_POINT ( 'NONE',  ( -11.35354668330684724, -30.33632613426204117, -2.999999999999971578 ) ) ;
#10512 = ADVANCED_FACE ( 'NONE', ( #21904, #13385, #11228, #9744, #18227 ), #21784, .T. ) ;
#10513 = TOROIDAL_SURFACE ( 'NONE', #5792, 34.90673715956759082, 8.750000000000000000 ) ;
#10514 = EDGE_LOOP ( 'NONE', ( #14035, #4916 ) ) ;
#10515 = CARTESIAN_POINT ( 'NONE',  ( 42.50000000000000711, -11.97499999999999964, -45.00000000000000000 ) ) ;
#10516 = AXIS2_PLACEMENT_3D ( 'NONE', #15915, #233, #21433 ) ;
#10517 = FACE_BOUND ( 'NONE', #22548, .T. ) ;
#10518 = CARTESIAN_POINT ( 'NONE',  ( 35.00000000000000711, 40.00000000000000000, -51.00000000000001421 ) ) ;
#10519 = PLANE ( 'NONE',  #1596 ) ;
#10520 = CIRCLE ( 'NONE', #20781, 49.99999999999998579 ) ;
#10521 = ORIENTED_EDGE ( 'NONE', *, *, #5445, .T. ) ;
#10522 = DIRECTION ( 'NONE',  ( -1.000000000000000000, -1.208970125616046080E-17, 6.505213034913038160E-19 ) ) ;
#10523 = CARTESIAN_POINT ( 'NONE',  ( -7.094908322883119567, 35.33352588067076283, -6.999999999999950262 ) ) ;
#10524 = EDGE_CURVE ( 'NONE', #19371, #14798, #18566, .T. ) ;
#10525 = VECTOR ( 'NONE', #17551, 1000.000000000000000 ) ;
#10526 = ORIENTED_EDGE ( 'NONE', *, *, #196, .T. ) ;
#10527 = AXIS2_PLACEMENT_3D ( 'NONE', #3831, #14114, #19193 ) ;
#10528 = AXIS2_PLACEMENT_3D ( 'NONE', #15161, #18737, #18851 ) ;
#10529 = ADVANCED_FACE ( 'NONE', ( #15219 ), #6200, .T. ) ;
#10530 = VECTOR ( 'NONE', #16522, 1000.000000000000000 ) ;
#10531 = ORIENTED_EDGE ( 'NONE', *, *, #16678, .F. ) ;
#10532 = CYLINDRICAL_SURFACE ( 'NONE', #14242, 15.00000000000000000 ) ;
#10533 = DIRECTION ( 'NONE',  ( 0.000000000000000000, 0.000000000000000000, -1.000000000000000000 ) ) ;
#10534 = DIRECTION ( 'NONE',  ( -0.000000000000000000, 1.000000000000000000, -0.000000000000000000 ) ) ;
#10535 = ORIENTED_EDGE ( 'NONE', *, *, #16432, .F. ) ;
#10536 = CYLINDRICAL_SURFACE ( 'NONE', #3262, 25.00000000000000711 ) ;
#10537 = CARTESIAN_POINT ( 'NONE',  ( -10.79056263833820850, 39.99999999999999289, -53.90082266129228827 ) ) ;
#10538 = ORIENTED_EDGE ( 'NONE', *, *, #4142, .T. ) ;
#10539 = DIRECTION ( 'NONE',  ( -0.000000000000000000, 1.000000000000000000, -0.000000000000000000 ) ) ;
#10540 = CARTESIAN_POINT ( 'NONE',  ( 22.08212374814979384, 16.07286297122273311, -58.59297470305927646 ) ) ;
#10541 = DIRECTION ( 'NONE',  ( -1.000000000000000000, 0.000000000000000000, 0.000000000000000000 ) ) ;
#10542 = CARTESIAN_POINT ( 'NONE',  ( -6.217947036537184502, 39.75326280012639302, -52.92450753908158845 ) ) ;
#10543 = AXIS2_PLACEMENT_3D ( 'NONE', #19218, #22429, #15525 ) ;
#10544 = ORIENTED_EDGE ( 'NONE', *, *, #14754, .F. ) ;
#10545 = CYLINDRICAL_SURFACE ( 'NONE', #2078, 0.9999999999999974465 ) ;
#10546 = CARTESIAN_POINT ( 'NONE',  ( -22.08212374814983292, 16.07286297122275798, 58.59297470305928357 ) ) ;
#10547 = B_SPLINE_CURVE_WITH_KNOTS ( 'NONE', 3,
 ( #2463, #275, #7498, #21254 ),
 .UNSPECIFIED., .F., .F.,
 ( 4, 4 ),
 ( 9.545285770017924652E-07, 0.001900595205834748483 ),
 .UNSPECIFIED. ) ;
#10548 = EDGE_LOOP ( 'NONE', ( #22434, #20899 ) ) ;
#10549 = CARTESIAN_POINT ( 'NONE',  ( 11.05758567242883572, 3.294696707135831737, 55.18338768059803812 ) ) ;
#10550 = AXIS2_PLACEMENT_3D ( 'NONE', #18430, #20050, #21651 ) ;
#10551 = DIRECTION ( 'NONE',  ( -1.000000000000000000, -1.208970125616081209E-17, 0.000000000000000000 ) ) ;
#10552 = DIRECTION ( 'NONE',  ( -6.505213034913038160E-19, -3.903127820947822896E-18, -1.000000000000000000 ) ) ;
#10553 = AXIS2_PLACEMENT_3D ( 'NONE', #21095, #2180, #17984 ) ;
#10554 = EDGE_CURVE ( 'NONE', #5122, #164, #16849, .T. ) ;
#10555 = ORIENTED_EDGE ( 'NONE', *, *, #10253, .F. ) ;
#10556 = ORIENTED_EDGE ( 'NONE', *, *, #8108, .T. ) ;
#10557 = VECTOR ( 'NONE', #12777, 1000.000000000000000 ) ;
#10558 = ORIENTED_EDGE ( 'NONE', *, *, #19075, .T. ) ;
#10559 = CIRCLE ( 'NONE', #22311, 60.00000000000000000 ) ;
#10560 = ADVANCED_FACE ( 'NONE', ( #22010 ), #11458, .T. ) ;
#10561 = EDGE_CURVE ( 'NONE', #5921, #4421, #1269, .T. ) ;
#10562 = EDGE_CURVE ( 'NONE', #18033, #2388, #7468, .T. ) ;
#10563 = ORIENTED_EDGE ( 'NONE', *, *, #11310, .F. ) ;
#10564 = CARTESIAN_POINT ( 'NONE',  ( -2.842671867355789139, 22.97192695149968955, 6.539645084693655797 ) ) ;
#10565 = CARTESIAN_POINT ( 'NONE',  ( 35.00000000000000000, 39.00000000000000711, -49.99999999999997868 ) ) ;
#10566 = DIRECTION ( 'NONE',  ( -0.000000000000000000, -1.000000000000000000, -0.000000000000000000 ) ) ;
#10567 = CARTESIAN_POINT ( 'NONE',  ( 2.220446049250313081E-13, -8.326672684688674053E-14, 2.800654218530498785 ) ) ;
#10568 = ORIENTED_EDGE ( 'NONE', *, *, #20591, .T. ) ;
#10569 = CARTESIAN_POINT ( 'NONE',  ( -1.387778780781445518E-14, 20.00000000000000355, -100.0000000000000000 ) ) ;
#10570 = CARTESIAN_POINT ( 'NONE',  ( 42.49999999999998579, 7.000000000000000000, -44.99999999999997868 ) ) ;
#10571 = EDGE_LOOP ( 'NONE', ( #16445, #1299, #14801, #12795, #1449 ) ) ;
#10572 = CARTESIAN_POINT ( 'NONE',  ( -31.88709182564680589, 6.070730550690766947, 2.999999999999995559 ) ) ;
#10573 = CARTESIAN_POINT ( 'NONE',  ( -30.60042966911723283, -7.474202570535854129, -2.999999999999971578 ) ) ;
#10574 = CARTESIAN_POINT ( 'NONE',  ( -13.67681338760606735, 37.77871559274755953, -56.08437820317177369 ) ) ;
#10575 = ORIENTED_EDGE ( 'NONE', *, *, #14311, .T. ) ;
#10576 = DIRECTION ( 'NONE',  ( -0.000000000000000000, -1.000000000000000000, -0.000000000000000000 ) ) ;
#10577 = ORIENTED_EDGE ( 'NONE', *, *, #7437, .F. ) ;
#10578 = FACE_OUTER_BOUND ( 'NONE', #9182, .T. ) ;
#10579 = EDGE_CURVE ( 'NONE', #11067, #17027, #10064, .T. ) ;
#10580 = CYLINDRICAL_SURFACE ( 'NONE', #13374, 10.00000000000000178 ) ;
#10581 = CARTESIAN_POINT ( 'NONE',  ( 35.00000000000000000, 14.00000000000000000, -38.99999999999997868 ) ) ;
#10582 = ADVANCED_FACE ( 'NONE', ( #8366, #4819, #10290, #3439, #13602, #15336, #10517, #19023 ), #15558, .T. ) ;
#10583 = CARTESIAN_POINT ( 'NONE',  ( 18.96886095803687056, 26.35434275172393015, 60.36758075326454787 ) ) ;
#10584 = DIRECTION ( 'NONE',  ( -0.000000000000000000, -0.000000000000000000, 1.000000000000000000 ) ) ;
#10585 = CARTESIAN_POINT ( 'NONE',  ( 3.460816278822046447E-15, -1.500000000000011768, 0.000000000000000000 ) ) ;
#10586 = ORIENTED_EDGE ( 'NONE', *, *, #1618, .T. ) ;
#10587 = ORIENTED_EDGE ( 'NONE', *, *, #3319, .F. ) ;
#10588 = EDGE_LOOP ( 'NONE', ( #1393, #17001, #15957, #17036 ) ) ;
#10589 = ORIENTED_EDGE ( 'NONE', *, *, #17660, .T. ) ;
#10590 = DIRECTION ( 'NONE',  ( -6.505213034913038160E-19, -3.903127820947822896E-18, -1.000000000000000000 ) ) ;
#10591 = DIRECTION ( 'NONE',  ( 0.000000000000000000, 0.000000000000000000, 1.000000000000000000 ) ) ;
#10592 = AXIS2_PLACEMENT_3D ( 'NONE', #9357, #21388, #9128 ) ;
#10593 = CARTESIAN_POINT ( 'NONE',  ( 35.00000000000000000, 22.00000000000000355, 2.365113165210053967E-14 ) ) ;
#10594 = CARTESIAN_POINT ( 'NONE',  ( 0.3971958550642871177, 39.99908967365433199, 49.04071034064279644 ) ) ;
#10595 = ADVANCED_FACE ( 'NONE', ( #15784 ), #11503, .F. ) ;
#10596 = EDGE_CURVE ( 'NONE', #18180, #16900, #13306, .T. ) ;
#10597 = ORIENTED_EDGE ( 'NONE', *, *, #14276, .T. ) ;
#10598 = CARTESIAN_POINT ( 'NONE',  ( -90.00000000000000000, 26.00000000000000355, -9.108981535246192915E-16 ) ) ;
#10599 = DIRECTION ( 'NONE',  ( -0.000000000000000000, 1.000000000000000000, -0.000000000000000000 ) ) ;
#10600 = CARTESIAN_POINT ( 'NONE',  ( -9.103081159019573931, 0.03030367950605317509, -53.87333532811887693 ) ) ;
#10601 = CARTESIAN_POINT ( 'NONE',  ( -32.83234229683721850, 11.85401191286866762, -2.999999999999971578 ) ) ;
#10602 = CIRCLE ( 'NONE', #4397, 31.50000000000000000 ) ;
#10603 = EDGE_CURVE ( 'NONE', #14814, #11530, #14404, .T. ) ;
#10604 = CARTESIAN_POINT ( 'NONE',  ( -11.50056215611671107, 36.46966885432792083, 57.85578624339548526 ) ) ;
#10605 = CARTESIAN_POINT ( 'NONE',  ( 35.00000000000002132, 0.000000000000000000, 58.99999999999701572 ) ) ;
#10606 = FACE_BOUND ( 'NONE', #12229, .T. ) ;
#10607 = DIRECTION ( 'NONE',  ( 1.296372316667914327E-16, 1.000000000000000000, -0.000000000000000000 ) ) ;
#10608 = ORIENTED_EDGE ( 'NONE', *, *, #9895, .F. ) ;
#10609 = EDGE_LOOP ( 'NONE', ( #2641, #8068, #5510, #8451 ) ) ;
#10610 = ORIENTED_EDGE ( 'NONE', *, *, #5667, .T. ) ;
#10611 = DIRECTION ( 'NONE',  ( 0.000000000000000000, -1.000000000000000000, 0.000000000000000000 ) ) ;
#10612 = AXIS2_PLACEMENT_3D ( 'NONE', #17619, #3766, #15886 ) ;
#10613 = DIRECTION ( 'NONE',  ( 0.000000000000000000, 0.000000000000000000, 1.000000000000000000 ) ) ;
#10614 = CARTESIAN_POINT ( 'NONE',  ( 4.000000000000003553, 1.499999999999994005, 4.898587196589412829E-16 ) ) ;
#10615 = PLANE ( 'NONE',  #18159 ) ;
#10616 = CARTESIAN_POINT ( 'NONE',  ( 9.103081159015154356, 0.03030367950454006254, 53.87333532811640424 ) ) ;
#10617 = MANIFOLD_SOLID_BREP ( 'Move Face1', #19217 ) ;
#10618 = CARTESIAN_POINT ( 'NONE',  ( 31.47226199422872028, -17.79229176513319288, -2.933296326616341876 ) ) ;
#10619 = PLANE ( 'NONE',  #21796 ) ;
#10620 = ORIENTED_EDGE ( 'NONE', *, *, #2034, .F. ) ;
#10621 = LINE ( 'NONE', #12243, #21118 ) ;
#10622 = CYLINDRICAL_SURFACE ( 'NONE', #5127, 2.499999999999998668 ) ;
#10623 = AXIS2_PLACEMENT_3D ( 'NONE', #15275, #9682, #11399 ) ;
#10624 = DIRECTION ( 'NONE',  ( 0.000000000000000000, 0.000000000000000000, 1.000000000000000000 ) ) ;
#10625 = CARTESIAN_POINT ( 'NONE',  ( 13.07600923154788219, 12.64060470162861272, -44.93756990742566160 ) ) ;
#10626 = ORIENTED_EDGE ( 'NONE', *, *, #12117, .F. ) ;
#10627 = CIRCLE ( 'NONE', #13560, 19.11328065563152023 ) ;
#10628 = CARTESIAN_POINT ( 'NONE',  ( -34.99999999999980815, 40.00000000000000000, 57.49999999999921840 ) ) ;
#10629 = LINE ( 'NONE', #11092, #14019 ) ;
#10630 = EDGE_CURVE ( 'NONE', #21858, #1751, #20616, .T. ) ;
#10631 = ORIENTED_EDGE ( 'NONE', *, *, #8073, .T. ) ;
#10632 = ADVANCED_FACE ( 'NONE', ( #10180, #17521, #6988, #18908 ), #13944, .F. ) ;
#10633 = AXIS2_PLACEMENT_3D ( 'NONE', #2837, #18870, #13230 ) ;
#10634 = EDGE_LOOP ( 'NONE', ( #15005, #1375, #946, #7211 ) ) ;
#10635 = CARTESIAN_POINT ( 'NONE',  ( 1.572625745562107991, 24.67014512736552945, 8.879522542764194171 ) ) ;
#10636 = DIRECTION ( 'NONE',  ( 0.000000000000000000, 0.000000000000000000, -1.000000000000000000 ) ) ;
#10637 = CARTESIAN_POINT ( 'NONE',  ( 0.003185071962414435728, 24.99999830921895594, 8.999999436406460163 ) ) ;
#10638 = VERTEX_POINT ( 'NONE', #20966 ) ;
#10639 = FACE_BOUND ( 'NONE', #368, .T. ) ;
#10640 = DIRECTION ( 'NONE',  ( -1.000000000000000000, 0.000000000000000000, 0.000000000000000000 ) ) ;
#10641 = ORIENTED_EDGE ( 'NONE', *, *, #21221, .T. ) ;
#10642 = CYLINDRICAL_SURFACE ( 'NONE', #248, 3.999999999999996447 ) ;
#10643 = CARTESIAN_POINT ( 'NONE',  ( 19.90072640592957853, 9.610007367499614261, -58.06946678856479593 ) ) ;
#10644 = DIRECTION ( 'NONE',  ( -0.1421319796954322034, 0.000000000000000000, -0.9898477157360405787 ) ) ;
#10645 = CARTESIAN_POINT ( 'NONE',  ( -12.24744603029287937, 40.00000000000000000, -54.43639671998464991 ) ) ;
#10646 = ORIENTED_EDGE ( 'NONE', *, *, #2498, .T. ) ;
#10647 = DIRECTION ( 'NONE',  ( -0.000000000000000000, 1.000000000000000000, -0.000000000000000000 ) ) ;
#10648 = CARTESIAN_POINT ( 'NONE',  ( -10.62139969368297443, 0.6004703193305642728, 54.70636795414677778 ) ) ;
#10649 = CARTESIAN_POINT ( 'NONE',  ( -4.573707352612297328, 39.86977586383432737, -51.94771487799405918 ) ) ;
#10650 = ORIENTED_EDGE ( 'NONE', *, *, #22489, .F. ) ;
#10651 = CIRCLE ( 'NONE', #16530, 10.00000000000000178 ) ;
#10652 = DIRECTION ( 'NONE',  ( 0.000000000000000000, 0.000000000000000000, -1.000000000000000000 ) ) ;
#10653 = CARTESIAN_POINT ( 'NONE',  ( -31.88709182564693378, 6.070730550690822902, -2.999999999999999112 ) ) ;
#10654 = MANIFOLD_SOLID_BREP ( 'Chamfer2', #6402 ) ;
#10655 = EDGE_CURVE ( 'NONE', #22114, #17215, #1997, .T. ) ;
#10656 = EDGE_LOOP ( 'NONE', ( #9560, #14306, #19115, #11443 ) ) ;
#10657 = EDGE_CURVE ( 'NONE', #16002, #12869, #7492, .T. ) ;
#10658 = ORIENTED_EDGE ( 'NONE', *, *, #15882, .T. ) ;
#10659 = ORIENTED_EDGE ( 'NONE', *, *, #8924, .F. ) ;
#10660 = ORIENTED_EDGE ( 'NONE', *, *, #2470, .T. ) ;
#10661 = LINE ( 'NONE', #7250, #15039 ) ;
#10662 = CIRCLE ( 'NONE', #12499, 59.99999999999703704 ) ;
#10663 = CARTESIAN_POINT ( 'NONE',  ( 4.198144980488468292, 39.89210059029527855, -51.71386871416487452 ) ) ;
#10664 = CARTESIAN_POINT ( 'NONE',  ( 6.607276003051461011, 39.99999999999998579, 52.37472748948959378 ) ) ;
#10665 = ORIENTED_EDGE ( 'NONE', *, *, #17326, .F. ) ;
#10666 = DIRECTION ( 'NONE',  ( 0.000000000000000000, -1.000000000000000000, 0.000000000000000000 ) ) ;
#10667 = CARTESIAN_POINT ( 'NONE',  ( -3.174475770749913828, -4.645331003331745201, -47.72510079650425752 ) ) ;
#10668 = ORIENTED_EDGE ( 'NONE', *, *, #1892, .F. ) ;
#10669 = CARTESIAN_POINT ( 'NONE',  ( 0.6841746959067585010, 36.75746821813302745, -2.800654218530457484 ) ) ;
#10670 = DIRECTION ( 'NONE',  ( 0.000000000000000000, -0.000000000000000000, 1.000000000000000000 ) ) ;
#10671 = FACE_OUTER_BOUND ( 'NONE', #4696, .T. ) ;
#10672 = ORIENTED_EDGE ( 'NONE', *, *, #19848, .F. ) ;
#10673 = ADVANCED_FACE ( 'NONE', ( #12356, #19579, #4008, #7200, #8917, #4112, #3890, #550 ), #15893, .F. ) ;
#10674 = CARTESIAN_POINT ( 'NONE',  ( 6.094635461695178336, 0.8905127700715224082, 54.73853566233531609 ) ) ;
#10675 = VERTEX_POINT ( 'NONE', #14400 ) ;
#10676 = CARTESIAN_POINT ( 'NONE',  ( 3.244689583147984280, 39.74755540027143752, -52.34195286441637052 ) ) ;
#10677 = CARTESIAN_POINT ( 'NONE',  ( -1.255208329926627453, 39.96308463907305253, 50.19868133818723521 ) ) ;
#10678 = SURFACE_SIDE_STYLE ('',( #2763 ) ) ;
#10679 = SURFACE_STYLE_FILL_AREA ( #19428 ) ;
#10680 = CARTESIAN_POINT ( 'NONE',  ( 8.835435312963896948, 40.00000000000000000, -53.27933556908502766 ) ) ;
#10681 = CARTESIAN_POINT ( 'NONE',  ( 20.00424115936584712, 19.83711385861052889, 60.62278039730742307 ) ) ;
#10682 = DIRECTION ( 'NONE',  ( 0.000000000000000000, 0.000000000000000000, 1.000000000000000000 ) ) ;
#10683 = EDGE_CURVE ( 'NONE', #862, #6172, #16257, .T. ) ;
#10684 = EDGE_CURVE ( 'NONE', #10193, #15500, #19368, .T. ) ;
#10685 = VECTOR ( 'NONE', #8694, 1000.000000000000000 ) ;
#10686 = VECTOR ( 'NONE', #7620, 1000.000000000000000 ) ;
#10687 = DIRECTION ( 'NONE',  ( 6.505213034913038160E-19, 3.903127820947822896E-18, 1.000000000000000000 ) ) ;
#10688 = CIRCLE ( 'NONE', #11795, 31.50000000000001421 ) ;
#10689 = VERTEX_POINT ( 'NONE', #206 ) ;
#10690 = VERTEX_POINT ( 'NONE', #14170 ) ;
#10691 = EDGE_CURVE ( 'NONE', #13427, #11968, #2313, .T. ) ;
#10692 = ORIENTED_EDGE ( 'NONE', *, *, #4580, .T. ) ;
#10693 = ORIENTED_EDGE ( 'NONE', *, *, #12137, .T. ) ;
#10694 = CARTESIAN_POINT ( 'NONE',  ( 2.999999999999997780, 15.99999999999999645, 8.485281374238567764 ) ) ;
#10695 = FACE_OUTER_BOUND ( 'NONE', #17272, .T. ) ;
#10696 = DIRECTION ( 'NONE',  ( 0.8171172023792293571, 0.3308262969263032760, -0.4720947350246252339 ) ) ;
#10697 = EDGE_CURVE ( 'NONE', #18519, #22383, #17738, .T. ) ;
#10698 = CARTESIAN_POINT ( 'NONE',  ( -35.00000000000058265, 40.00000000000000711, -52.47500000000076170 ) ) ;
#10699 = DIRECTION ( 'NONE',  ( -0.000000000000000000, -1.000000000000000000, -0.000000000000000000 ) ) ;
#10700 = CARTESIAN_POINT ( 'NONE',  ( 0.2316811374357567177, 39.99968400796328893, 48.91347626078281507 ) ) ;
#10701 = B_SPLINE_CURVE_WITH_KNOTS ( 'NONE', 3,
 ( #14143, #5466, #3751, #7521, #14260, #2364 ),
 .UNSPECIFIED., .F., .F.,
 ( 4, 2, 4 ),
 ( 0.000000000000000000, 0.002641318319677474300, 0.005282636639354948600 ),
 .UNSPECIFIED. ) ;
#10702 = CIRCLE ( 'NONE', #11804, 11.99999999999999822 ) ;
#10703 = AXIS2_PLACEMENT_3D ( 'NONE', #19328, #22668, #13912 ) ;
#10704 = EDGE_CURVE ( 'NONE', #8676, #21259, #6394, .T. ) ;
#10705 = VERTEX_POINT ( 'NONE', #12457 ) ;
#10706 = FACE_OUTER_BOUND ( 'NONE', #15082, .T. ) ;
#10707 = CARTESIAN_POINT ( 'NONE',  ( -9.999999999999998224, 12.49999999999999822, 3.000000000000000000 ) ) ;
#10708 = DIRECTION ( 'NONE',  ( 0.000000000000000000, 1.000000000000000000, 0.000000000000000000 ) ) ;
#10709 = DIRECTION ( 'NONE',  ( 0.000000000000000000, 0.000000000000000000, -1.000000000000000000 ) ) ;
#10710 = VECTOR ( 'NONE', #20777, 1000.000000000000000 ) ;
#10711 = DIRECTION ( 'NONE',  ( -0.000000000000000000, 1.000000000000000000, -0.000000000000000000 ) ) ;
#10712 = ADVANCED_FACE ( 'NONE', ( #16016 ), #22132, .T. ) ;
#10713 = CARTESIAN_POINT ( 'NONE',  ( -1.387778780781445676E-14, 20.00000000000000000, -105.0020000000000095 ) ) ;
#10714 = CARTESIAN_POINT ( 'NONE',  ( -23.74488952252773544, 25.58633464742632313, 3.000000000000023537 ) ) ;
#10715 = EDGE_CURVE ( 'NONE', #5289, #14267, #14284, .T. ) ;
#10716 = VERTEX_POINT ( 'NONE', #17966 ) ;
#10717 = VECTOR ( 'NONE', #15038, 1000.000000000000000 ) ;
#10718 = EDGE_LOOP ( 'NONE', ( #8319, #1252 ) ) ;
#10719 = EDGE_CURVE ( 'NONE', #20208, #9999, #13679, .T. ) ;
#10720 = AXIS2_PLACEMENT_3D ( 'NONE', #8368, #6990, #22356 ) ;
#10721 = AXIS2_PLACEMENT_3D ( 'NONE', #8371, #6649, #6994 ) ;
#10722 = EDGE_LOOP ( 'NONE', ( #18896, #9923 ) ) ;
#10723 = CARTESIAN_POINT ( 'NONE',  ( 3.309563215936520475, -3.140776953251411374, -49.61090469809367676 ) ) ;
#10724 = EDGE_CURVE ( 'NONE', #11124, #18161, #14517, .T. ) ;
#10725 = EDGE_CURVE ( 'NONE', #17205, #8364, #5251, .T. ) ;
#10726 = CARTESIAN_POINT ( 'NONE',  ( -30.33632613426162550, 11.35354668330676375, 2.999999999999995559 ) ) ;
#10727 = FACE_OUTER_BOUND ( 'NONE', #2453, .T. ) ;
#10728 = AXIS2_PLACEMENT_3D ( 'NONE', #12998, #20017, #11300 ) ;
#10729 = DIRECTION ( 'NONE',  ( -0.5840452403773163104, 0.8117211080122304079, 0.000000000000000000 ) ) ;
#10730 = DIRECTION ( 'NONE',  ( -0.000000000000000000, -0.000000000000000000, -1.000000000000000000 ) ) ;
#10731 = CARTESIAN_POINT ( 'NONE',  ( -35.00000000000000000, 22.00000000000000711, 15.00000000000002132 ) ) ;
#10732 = DIRECTION ( 'NONE',  ( 1.000000000000000000, 0.000000000000000000, 0.000000000000000000 ) ) ;
#10733 = ORIENTED_EDGE ( 'NONE', *, *, #20824, .T. ) ;
#10734 = DIRECTION ( 'NONE',  ( 6.505213034913038160E-19, 3.903127820947822896E-18, 1.000000000000000000 ) ) ;
#10735 =( NAMED_UNIT ( * ) SI_UNIT ( $, .STERADIAN. ) SOLID_ANGLE_UNIT ( ) );
#10736 = AXIS2_PLACEMENT_3D ( 'NONE', #18311, #21877, #2629 ) ;
#10737 = DIRECTION ( 'NONE',  ( 0.000000000000000000, 0.000000000000000000, -1.000000000000000000 ) ) ;
#10738 = DIRECTION ( 'NONE',  ( 0.000000000000000000, -1.000000000000000000, 0.000000000000000000 ) ) ;
#10739 = AXIS2_PLACEMENT_3D ( 'NONE', #8947, #16273, #584 ) ;
#10740 = VERTEX_POINT ( 'NONE', #14347 ) ;
#10741 = DIRECTION ( 'NONE',  ( -1.296372316667914327E-16, -1.000000000000000000, 0.000000000000000000 ) ) ;
#10742 = CARTESIAN_POINT ( 'NONE',  ( -12.99999999999980282, -2.516660498395516310, -105.0000000000000142 ) ) ;
#10743 = EDGE_CURVE ( 'NONE', #3040, #1608, #10395, .T. ) ;
#10744 = CARTESIAN_POINT ( 'NONE',  ( 16.35275686153459063, 4.590993025984193565, -57.03319805596824921 ) ) ;
#10745 = CIRCLE ( 'NONE', #11132, 31.50000000000001421 ) ;
#10746 = VERTEX_POINT ( 'NONE', #9328 ) ;
#10747 = ADVANCED_FACE ( 'NONE', ( #21250 ), #5595, .F. ) ;
#10748 = CIRCLE ( 'NONE', #8580, 0.9999999999999974465 ) ;
#10749 = VERTEX_POINT ( 'NONE', #12415 ) ;
#10750 = CARTESIAN_POINT ( 'NONE',  ( -90.00000000000000000, 40.00000000000000000, -9.108981535246192915E-16 ) ) ;
#10751 = CARTESIAN_POINT ( 'NONE',  ( 7.310544252644470693E-15, 28.19616000222403684, 0.000000000000000000 ) ) ;
#10752 = CARTESIAN_POINT ( 'NONE',  ( 20.17230487860832611, 25.34312177887321127, 3.000000000000009770 ) ) ;
#10753 = VERTEX_POINT ( 'NONE', #2224 ) ;
#10754 = FACE_OUTER_BOUND ( 'NONE', #4695, .T. ) ;
#10755 = CARTESIAN_POINT ( 'NONE',  ( -8.550503583141882302, 23.49231551964767206, -5.000000000000004441 ) ) ;
#10756 = ORIENTED_EDGE ( 'NONE', *, *, #18807, .T. ) ;
#10757 = DIRECTION ( 'NONE',  ( -1.000000000000000000, -3.564803380056654458E-15, 0.000000000000000000 ) ) ;
#10758 = EDGE_CURVE ( 'NONE', #13475, #11887, #21355, .T. ) ;
#10759 = CARTESIAN_POINT ( 'NONE',  ( -35.00000000000000000, 38.99999999999999289, 1.387778780781445676E-14 ) ) ;
#10760 = CYLINDRICAL_SURFACE ( 'NONE', #4845, 19.11328065563151313 ) ;
#10761 = EDGE_LOOP ( 'NONE', ( #11696, #14892, #20306, #5418 ) ) ;
#10762 = DIRECTION ( 'NONE',  ( -1.000000000000000000, 0.000000000000000000, 0.000000000000000000 ) ) ;
#10763 = VECTOR ( 'NONE', #6510, 1000.000000000000000 ) ;
#10764 = CYLINDRICAL_SURFACE ( 'NONE', #10739, 2.999999999999999112 ) ;
#10765 = CARTESIAN_POINT ( 'NONE',  ( -1.103251808850783888, 39.99275656215084496, -49.57314659356683251 ) ) ;
#10766 = CIRCLE ( 'NONE', #9339, 19.11328065563151668 ) ;
#10767 = ORIENTED_EDGE ( 'NONE', *, *, #13298, .T. ) ;
#10768 = EDGE_CURVE ( 'NONE', #5161, #8683, #10351, .T. ) ;
#10769 = CARTESIAN_POINT ( 'NONE',  ( 3.330669073875469621E-13, -1.110223024625156540E-13, -2.999999999999971578 ) ) ;
#10770 = CARTESIAN_POINT ( 'NONE',  ( 34.74700806321118307, -12.00937115242653519, -2.800654218530457484 ) ) ;
#10771 = B_SPLINE_CURVE_WITH_KNOTS ( 'NONE', 3,
 ( #12986, #18379, #9566, #20339 ),
 .UNSPECIFIED., .F., .F.,
 ( 4, 4 ),
 ( 0.001875451646903067990, 0.003761979286331190026 ),
 .UNSPECIFIED. ) ;
#10772 = VECTOR ( 'NONE', #14804, 1000.000000000000000 ) ;
#10773 = ORIENTED_EDGE ( 'NONE', *, *, #5478, .F. ) ;
#10774 = CIRCLE ( 'NONE', #919, 16.49999999999998579 ) ;
#10775 = ORIENTED_EDGE ( 'NONE', *, *, #22554, .F. ) ;
#10776 = CIRCLE ( 'NONE', #15495, 2.500000000000002220 ) ;
#10777 = B_SPLINE_CURVE_WITH_KNOTS ( 'NONE', 3,
 ( #19888, #4199, #18171, #9471 ),
 .UNSPECIFIED., .F., .F.,
 ( 4, 4 ),
 ( 0.000000000000000000, 1.000000000000000000 ),
 .UNSPECIFIED. ) ;
#10778 = ORIENTED_EDGE ( 'NONE', *, *, #21736, .T. ) ;
#10779 = ORIENTED_EDGE ( 'NONE', *, *, #815, .T. ) ;
#10780 = FACE_OUTER_BOUND ( 'NONE', #1005, .T. ) ;
#10781 = B_SPLINE_CURVE_WITH_KNOTS ( 'NONE', 3,
 ( #15108, #18340, #2769, #2993 ),
 .UNSPECIFIED., .F., .F.,
 ( 4, 4 ),
 ( 0.001893031756885368063, 0.003808480026563666569 ),
 .UNSPECIFIED. ) ;
#10782 = AXIS2_PLACEMENT_3D ( 'NONE', #19806, #11079, #18069 ) ;
#10783 = CARTESIAN_POINT ( 'NONE',  ( 35.00000000000000000, 15.00000000000000000, 2.365113165210053967E-14 ) ) ;
#10784 = CARTESIAN_POINT ( 'NONE',  ( 1.571409433144389078, 40.00000000000000711, -49.72695173164139959 ) ) ;
#10785 = CARTESIAN_POINT ( 'NONE',  ( 9.519381200825437261, 39.99999999999999289, 53.51361895441421979 ) ) ;
#10786 = ORIENTED_EDGE ( 'NONE', *, *, #13408, .T. ) ;
#10787 = DIRECTION ( 'NONE',  ( -0.000000000000000000, -1.000000000000000000, -0.000000000000000000 ) ) ;
#10788 = DIRECTION ( 'NONE',  ( -1.000000000000000000, 0.000000000000000000, 0.000000000000000000 ) ) ;
#10789 = ORIENTED_EDGE ( 'NONE', *, *, #15067, .F. ) ;
#10790 = CARTESIAN_POINT ( 'NONE',  ( 25.00000000000000000, -20.00000000000000000, -16.49999999999997868 ) ) ;
#10791 = ADVANCED_FACE ( 'NONE', ( #7493 ), #12754, .T. ) ;
#10792 = CARTESIAN_POINT ( 'NONE',  ( 34.24928931925769149, -6.742883674876604339, 3.000000000000002665 ) ) ;
#10793 = DIRECTION ( 'NONE',  ( -0.000000000000000000, 1.000000000000000000, -0.000000000000000000 ) ) ;
#10794 = ORIENTED_EDGE ( 'NONE', *, *, #13116, .T. ) ;
#10795 = CARTESIAN_POINT ( 'NONE',  ( 34.74700806321121149, -12.00937115242670039, 2.800654218530512551 ) ) ;
#10796 = ORIENTED_EDGE ( 'NONE', *, *, #18338, .T. ) ;
#10797 = DIRECTION ( 'NONE',  ( 0.000000000000000000, 1.000000000000000000, 0.000000000000000000 ) ) ;
#10798 = VECTOR ( 'NONE', #11946, 1000.000000000000000 ) ;
#10799 = FACE_OUTER_BOUND ( 'NONE', #5812, .T. ) ;
#10800 = CARTESIAN_POINT ( 'NONE',  ( 42.50000000000000711, -11.97499999999999964, -50.00000000000000000 ) ) ;
#10801 = DIRECTION ( 'NONE',  ( -1.000000000000000000, 1.530638361156006492E-16, 0.000000000000000000 ) ) ;
#10802 = EDGE_CURVE ( 'NONE', #18491, #2692, #18145, .T. ) ;
#10803 = VECTOR ( 'NONE', #21664, 1000.000000000000000 ) ;
#10804 = CARTESIAN_POINT ( 'NONE',  ( 2.220446049250313081E-13, -8.326672684688674053E-14, 2.800654218530498785 ) ) ;
#10805 = CARTESIAN_POINT ( 'NONE',  ( 18.56336306567978411, 12.50537704746338541, 60.26262883998656150 ) ) ;
#10806 = CARTESIAN_POINT ( 'NONE',  ( -12.99999999999980282, -2.516660498395516310, 60.00099999999999767 ) ) ;
#10807 = CIRCLE ( 'NONE', #6800, 1.000000000000000888 ) ;
#10808 = DIRECTION ( 'NONE',  ( 1.000000000000000000, 0.000000000000000000, 0.000000000000000000 ) ) ;
#10809 = VERTEX_POINT ( 'NONE', #5540 ) ;
#10810 = ORIENTED_EDGE ( 'NONE', *, *, #5568, .T. ) ;
#10811 = EDGE_CURVE ( 'NONE', #11727, #16638, #6753, .T. ) ;
#10812 = ORIENTED_EDGE ( 'NONE', *, *, #9794, .F. ) ;
#10813 = AXIS2_PLACEMENT_3D ( 'NONE', #13895, #3061, #10032 ) ;
#10814 = AXIS2_PLACEMENT_3D ( 'NONE', #16450, #759, #14712 ) ;
#10815 = ORIENTED_EDGE ( 'NONE', *, *, #8080, .T. ) ;
#10816 = DIRECTION ( 'NONE',  ( -0.000000000000000000, 1.000000000000000000, -0.000000000000000000 ) ) ;
#10817 = FACE_OUTER_BOUND ( 'NONE', #17458, .T. ) ;
#10818 = CIRCLE ( 'NONE', #15193, 2.099999999999997868 ) ;
#10819 = DIRECTION ( 'NONE',  ( 0.000000000000000000, 0.000000000000000000, -1.000000000000000000 ) ) ;
#10820 = CARTESIAN_POINT ( 'NONE',  ( -31.41173278719236350, -17.66631876130928092, -6.999999999999950262 ) ) ;
#10821 = DIRECTION ( 'NONE',  ( -1.000000000000000000, -1.208970125616077665E-17, 0.000000000000000000 ) ) ;
#10822 = EDGE_CURVE ( 'NONE', #21718, #10976, #15756, .T. ) ;
#10823 = AXIS2_PLACEMENT_3D ( 'NONE', #20158, #11333, #14746 ) ;
#10824 = VERTEX_POINT ( 'NONE', #5775 ) ;
#10825 = LINE ( 'NONE', #15863, #4718 ) ;
#10826 = DIRECTION ( 'NONE',  ( 0.000000000000000000, 1.000000000000000000, 0.000000000000000000 ) ) ;
#10827 = CARTESIAN_POINT ( 'NONE',  ( -35.16985127952398926, -10.70799354677417980, 2.800654218530485018 ) ) ;
#10828 = DIRECTION ( 'NONE',  ( 0.000000000000000000, 0.000000000000000000, -1.000000000000000000 ) ) ;
#10829 = LINE ( 'NONE', #12884, #13509 ) ;
#10830 = VECTOR ( 'NONE', #6329, 1000.000000000000000 ) ;
#10831 = VECTOR ( 'NONE', #2502, 1000.000000000000000 ) ;
#10832 = AXIS2_PLACEMENT_3D ( 'NONE', #8503, #22496, #15252 ) ;
#10833 = DIRECTION ( 'NONE',  ( 1.000000000000000000, 1.208970125616063182E-17, 0.000000000000000000 ) ) ;
#10834 = CIRCLE ( 'NONE', #221, 2.000000000000001776 ) ;
#10835 = FACE_BOUND ( 'NONE', #3244, .T. ) ;
#10836 = CARTESIAN_POINT ( 'NONE',  ( 11.86180952234342278, 38.99999999999291589, -55.35904751185374550 ) ) ;
#10837 = ORIENTED_EDGE ( 'NONE', *, *, #19112, .T. ) ;
#10838 = CIRCLE ( 'NONE', #15230, 0.9999999999999974465 ) ;
#10839 = ORIENTED_EDGE ( 'NONE', *, *, #6806, .F. ) ;
#10840 = EDGE_CURVE ( 'NONE', #6249, #14950, #8666, .T. ) ;
#10841 = ORIENTED_EDGE ( 'NONE', *, *, #13589, .T. ) ;
#10842 = CARTESIAN_POINT ( 'NONE',  ( -34.99999999999980815, 28.00000000000000000, 54.99999999999922551 ) ) ;
#10843 = FACE_OUTER_BOUND ( 'NONE', #6371, .T. ) ;
#10844 = ADVANCED_FACE ( 'NONE', ( #616 ), #474, .T. ) ;
#10845 = EDGE_CURVE ( 'NONE', #15853, #4344, #12580, .T. ) ;
#10846 = CONICAL_SURFACE ( 'NONE', #5744, 57.00000000000002132, 0.7853981633974437271 ) ;
#10847 = ADVANCED_FACE ( 'NONE', ( #19529 ), #4174, .F. ) ;
#10848 = CYLINDRICAL_SURFACE ( 'NONE', #4787, 31.50000000000001421 ) ;
#10849 = CARTESIAN_POINT ( 'NONE',  ( 0.000000000000000000, 30.00000000000000000, 3.399999999999995026 ) ) ;
#10850 = CARTESIAN_POINT ( 'NONE',  ( -11.68090480754633553, 3.765577839755389622, 57.90797000640144176 ) ) ;
#10851 = MANIFOLD_SOLID_BREP ( 'M8 Tapped Hole3', #19569 ) ;
#10852 = CARTESIAN_POINT ( 'NONE',  ( -14.30947201679070346, 34.00909065834211731, -56.34794761833929044 ) ) ;
#10853 = DIRECTION ( 'NONE',  ( -0.000000000000000000, 1.000000000000000000, -0.000000000000000000 ) ) ;
#10854 = VECTOR ( 'NONE', #8863, 1000.000000000000000 ) ;
#10855 = ORIENTED_EDGE ( 'NONE', *, *, #10401, .F. ) ;
#10856 = CARTESIAN_POINT ( 'NONE',  ( -23.50000000000001066, 19.99999999999982947, 105.0000000000000142 ) ) ;
#10857 = EDGE_CURVE ( 'NONE', #4421, #4117, #14367, .T. ) ;
#10858 = CARTESIAN_POINT ( 'NONE',  ( -42.50000000000000711, -5.000000000000000000, -45.40000000000000568 ) ) ;
#10859 = CARTESIAN_POINT ( 'NONE',  ( 14.94062893683334003, 18.45609313704557763, -45.79998742252195143 ) ) ;
#10860 = EDGE_LOOP ( 'NONE', ( #2583, #19877, #17019, #18528 ) ) ;
#10861 = DIRECTION ( 'NONE',  ( 1.000000000000000000, -1.296372316667914327E-16, 0.000000000000000000 ) ) ;
#10862 = AXIS2_PLACEMENT_3D ( 'NONE', #15127, #9544, #13407 ) ;
#10863 = PLANE ( 'NONE',  #10368 ) ;
#10864 = AXIS2_PLACEMENT_3D ( 'NONE', #21888, #1022, #4470 ) ;
#10865 = DIRECTION ( 'NONE',  ( 0.000000000000000000, -1.000000000000000000, 0.000000000000000000 ) ) ;
#10866 = EDGE_LOOP ( 'NONE', ( #1328, #9531, #20927, #19129, #21430, #21422 ) ) ;
#10867 = AXIS2_PLACEMENT_3D ( 'NONE', #15234, #11592, #940 ) ;
#10868 = CONTEXT_DEPENDENT_SHAPE_REPRESENTATION ( #2442, #19915 ) ;
#10869 = ORIENTED_EDGE ( 'NONE', *, *, #10208, .T. ) ;
#10870 = CARTESIAN_POINT ( 'NONE',  ( -2.999999999999998668, 22.79887287893604153, 8.485281374238567764 ) ) ;
#10871 = B_SPLINE_CURVE_WITH_KNOTS ( 'NONE', 3,
 ( #15158, #381, #17455, #22035 ),
 .UNSPECIFIED., .F., .F.,
 ( 4, 4 ),
 ( 0.001893031756885371316, 0.003808480026563539934 ),
 .UNSPECIFIED. ) ;
#10872 = AXIS2_PLACEMENT_3D ( 'NONE', #17419, #13863, #3690 ) ;
#10873 = CARTESIAN_POINT ( 'NONE',  ( -9.857944917841395593, 0.2919354798322454925, 54.29891737064847490 ) ) ;
#10874 = FACE_OUTER_BOUND ( 'NONE', #11100, .T. ) ;
#10875 = VECTOR ( 'NONE', #7880, 1000.000000000000000 ) ;
#10876 = ORIENTED_EDGE ( 'NONE', *, *, #331, .T. ) ;
#10877 = FACE_BOUND ( 'NONE', #3148, .T. ) ;
#10878 = CARTESIAN_POINT ( 'NONE',  ( -5.863456460679469018, 40.00000000000000000, 52.03112161586459194 ) ) ;
#10879 = ORIENTED_EDGE ( 'NONE', *, *, #19405, .F. ) ;
#10880 = DIRECTION ( 'NONE',  ( 6.505213034913038160E-19, 3.903127820947822896E-18, 1.000000000000000000 ) ) ;
#10881 = LINE ( 'NONE', #16144, #7960 ) ;
#10882 = AXIS2_PLACEMENT_3D ( 'NONE', #20603, #4699, #11675 ) ;
#10883 = EDGE_CURVE ( 'NONE', #17279, #4759, #22069, .T. ) ;
#10884 = CARTESIAN_POINT ( 'NONE',  ( 6.696867368503558448E-15, 40.00000000000000000, 48.73397172404481381 ) ) ;
#10885 = EDGE_CURVE ( 'NONE', #768, #7786, #21702, .T. ) ;
#10886 = DIRECTION ( 'NONE',  ( 6.505213034913038160E-19, 3.903127820947822896E-18, 1.000000000000000000 ) ) ;
#10887 = ORIENTED_EDGE ( 'NONE', *, *, #21284, .T. ) ;
#10888 = CARTESIAN_POINT ( 'NONE',  ( -34.90673715956753398, -1.391998901022310567E-13, -5.749999999999949374 ) ) ;
#10889 = DIRECTION ( 'NONE',  ( 1.000000000000000000, -1.084202172485504434E-16, 0.000000000000000000 ) ) ;
#10890 = CARTESIAN_POINT ( 'NONE',  ( -6.675595700168979185, 39.71118686595398373, -53.17234509353112770 ) ) ;
#10891 = EDGE_LOOP ( 'NONE', ( #1831, #12485, #15068 ) ) ;
#10892 = VECTOR ( 'NONE', #709, 1000.000000000000000 ) ;
#10893 = EDGE_CURVE ( 'NONE', #21392, #9227, #9778, .T. ) ;
#10894 = LINE ( 'NONE', #19501, #9361 ) ;
#10895 = DIRECTION ( 'NONE',  ( 6.505213034913038160E-19, 3.903127820947822896E-18, 1.000000000000000000 ) ) ;
#10896 = CIRCLE ( 'NONE', #8711, 59.99999999999700862 ) ;
#10897 = B_SPLINE_CURVE_WITH_KNOTS ( 'NONE', 3,
 ( #19416, #42, #10234, #6932, #7138, #12298, #10453, #12186, #17452, #17569, #6813, #17341 ),
 .UNSPECIFIED., .F., .F.,
 ( 4, 2, 2, 2, 2, 4 ),
 ( 0.006347202264228479079, 0.007930096811551054850, 0.008721544085212341868, 0.009512991358873628886, 0.01109588590619620986, 0.01267878045351878910 ),
 .UNSPECIFIED. ) ;
#10898 = VECTOR ( 'NONE', #1317, 1000.000000000000000 ) ;
#10899 = VECTOR ( 'NONE', #22544, 1000.000000000000000 ) ;
#10900 = VERTEX_POINT ( 'NONE', #19985 ) ;
#10901 = VERTEX_POINT ( 'NONE', #956 ) ;
#10902 = ORIENTED_EDGE ( 'NONE', *, *, #443, .T. ) ;
#10903 = EDGE_LOOP ( 'NONE', ( #19092, #22276, #20592 ) ) ;
#10904 = DIRECTION ( 'NONE',  ( -1.000000000000000000, 0.000000000000000000, 0.000000000000000000 ) ) ;
#10905 = CARTESIAN_POINT ( 'NONE',  ( 2.220446049250313081E-13, 2.775557561562891351E-14, -2.800654218530485018 ) ) ;
#10906 = CARTESIAN_POINT ( 'NONE',  ( 35.00000000000000000, 40.00000000000000000, 4.258610482196280173E-15 ) ) ;
#10907 = SHAPE_REPRESENTATION ( 'SEAL', ( #18273 ), #5109 ) ;
#10908 = VECTOR ( 'NONE', #8478, 1000.000000000000000 ) ;
#10909 = ORIENTED_EDGE ( 'NONE', *, *, #21208, .T. ) ;
#10910 = CARTESIAN_POINT ( 'NONE',  ( 2.220446049250313081E-13, 2.775557561562891351E-14, -2.800654218530485018 ) ) ;
#10911 = CARTESIAN_POINT ( 'NONE',  ( -21.00948735876860596, -24.79619811426211839, 2.999999999999995559 ) ) ;
#10912 = VERTEX_POINT ( 'NONE', #16651 ) ;
#10913 = CARTESIAN_POINT ( 'NONE',  ( -34.24928931925764886, 6.742883674876548383, 2.999999999999999112 ) ) ;
#10914 = LINE ( 'NONE', #9199, #8282 ) ;
#10915 = AXIS2_PLACEMENT_3D ( 'NONE', #516, #4085, #16446 ) ;
#10916 = CARTESIAN_POINT ( 'NONE',  ( 23.74488952252801255, -25.58633464742643326, -2.999999999999978240 ) ) ;
#10917 = VERTEX_POINT ( 'NONE', #4750 ) ;
#10918 = DIRECTION ( 'NONE',  ( 6.505213034913038160E-19, 3.903127820947822896E-18, 1.000000000000000000 ) ) ;
#10919 = ORIENTED_EDGE ( 'NONE', *, *, #8501, .T. ) ;
#10920 = CARTESIAN_POINT ( 'NONE',  ( 3.630528349514350772, 39.68566064946332972, -51.94954034995315340 ) ) ;
#10921 = CARTESIAN_POINT ( 'NONE',  ( 42.50000000000000711, -5.000000000000000000, 47.50000000000000711 ) ) ;
#10922 = CIRCLE ( 'NONE', #10176, 9.000000000000003553 ) ;
#10923 = DIRECTION ( 'NONE',  ( 0.000000000000000000, 0.000000000000000000, -1.000000000000000000 ) ) ;
#10924 = EDGE_LOOP ( 'NONE', ( #13973, #22029, #14506, #18324, #19021, #7893 ) ) ;
#10925 = DIRECTION ( 'NONE',  ( 6.505213034913038160E-19, 3.903127820947822896E-18, 1.000000000000000000 ) ) ;
#10926 = CARTESIAN_POINT ( 'NONE',  ( 17.83677152930479082, 10.91058841726731998, 60.06362461869429126 ) ) ;
#10927 = CARTESIAN_POINT ( 'NONE',  ( 27.19760187735878532, 24.73600648735102681, -2.800654218530485018 ) ) ;
#10928 = CARTESIAN_POINT ( 'NONE',  ( 13.71171267332174715, 34.59605702017176299, -56.12298047978914894 ) ) ;
#10929 = CIRCLE ( 'NONE', #5459, 1.000000000000000888 ) ;
#10930 = CIRCLE ( 'NONE', #12036, 5.000000000000000000 ) ;
#10932 = ORIENTED_EDGE ( 'NONE', *, *, #15182, .T. ) ;
#10931 = ADVANCED_FACE ( 'NONE', ( #16768 ), #3307, .F. ) ;
#10933 = ORIENTED_EDGE ( 'NONE', *, *, #16176, .T. ) ;
#10934 = ORIENTED_EDGE ( 'NONE', *, *, #903, .T. ) ;
#10935 = PRODUCT_DEFINITION_FORMATION_WITH_SPECIFIED_SOURCE ( 'ANY', '', #17518, .NOT_KNOWN. ) ;
#10936 = ORIENTED_EDGE ( 'NONE', *, *, #11175, .T. ) ;
#10937 = FACE_OUTER_BOUND ( 'NONE', #18926, .T. ) ;
#10938 = EDGE_CURVE ( 'NONE', #17505, #17561, #15516, .T. ) ;
#10939 = CARTESIAN_POINT ( 'NONE',  ( -10.44987231380843618, 39.22455541072930174, -54.81340832922769124 ) ) ;
#10940 = EDGE_CURVE ( 'NONE', #18457, #15515, #20890, .T. ) ;
#10941 = PRODUCT ( 'GEAR', 'GEAR', '', ( #10410 ) ) ;
#10942 = LINE ( 'NONE', #21376, #4177 ) ;
#10943 = ORIENTED_EDGE ( 'NONE', *, *, #20503, .F. ) ;
#10944 = CYLINDRICAL_SURFACE ( 'NONE', #14578, 19.11328065563152379 ) ;
#10945 = CARTESIAN_POINT ( 'NONE',  ( 15.12081897056688540, -33.51030287062373247, 2.800654218530485018 ) ) ;
#10946 = COLOUR_RGB ( '',0.7921568627450980005, 0.8196078431372548767, 0.9333333333333333481 ) ;
#10947 = VERTEX_POINT ( 'NONE', #17315 ) ;
#10948 = FACE_OUTER_BOUND ( 'NONE', #6523, .T. ) ;
#10949 = PRODUCT_DEFINITION_CONTEXT ( 'detailed design', #11506, 'design' ) ;
#10950 = CARTESIAN_POINT ( 'NONE',  ( 7.310544252644470693E-15, 28.19616000222403684, 0.000000000000000000 ) ) ;
#10951 = DIRECTION ( 'NONE',  ( 0.000000000000000000, 0.000000000000000000, 1.000000000000000000 ) ) ;
#10952 =( NAMED_UNIT ( * ) SI_UNIT ( $, .STERADIAN. ) SOLID_ANGLE_UNIT ( ) );
#10953 = EDGE_CURVE ( 'NONE', #4765, #16523, #3249, .T. ) ;
#10954 = LINE ( 'NONE', #17831, #20492 ) ;
#10955 = CARTESIAN_POINT ( 'NONE',  ( -5.133465198558034182, 39.34078186380426700, 53.02544092942117970 ) ) ;
#10956 = FACE_OUTER_BOUND ( 'NONE', #1594, .T. ) ;
#10957 = EDGE_CURVE ( 'NONE', #16727, #9194, #170, .T. ) ;
#10958 = EDGE_LOOP ( 'NONE', ( #9116, #19137, #15021, #5435 ) ) ;
#10959 = ORIENTED_EDGE ( 'NONE', *, *, #11589, .T. ) ;
#10960 = VECTOR ( 'NONE', #15869, 1000.000000000000000 ) ;
#10961 = EDGE_LOOP ( 'NONE', ( #18458, #10577, #12982, #18087 ) ) ;
#10962 = EDGE_CURVE ( 'NONE', #19759, #10205, #10748, .T. ) ;
#10963 = DIRECTION ( 'NONE',  ( -0.000000000000000000, -1.000000000000000000, -0.000000000000000000 ) ) ;
#10964 = CARTESIAN_POINT ( 'NONE',  ( 42.50000000000000711, -5.000000000000000000, -45.40000000000000568 ) ) ;
#10965 = CARTESIAN_POINT ( 'NONE',  ( -35.99819890246953946, 7.463862311151231665, 2.800654218530509443 ) ) ;
#10966 = CIRCLE ( 'NONE', #11337, 9.000000000000003553 ) ;
#10967 = DIRECTION ( 'NONE',  ( -1.000000000000000000, -1.208970125616060101E-17, 6.505213034913038160E-19 ) ) ;
#10968 = FACE_OUTER_BOUND ( 'NONE', #11330, .T. ) ;
#10969 = CARTESIAN_POINT ( 'NONE',  ( -42.50000000000000000, 10.00000000000000000, 44.99999999999999289 ) ) ;
#10970 = CARTESIAN_POINT ( 'NONE',  ( -19.95262135541531379, 18.40707545474674589, 60.61067493606138612 ) ) ;
#10971 = CARTESIAN_POINT ( 'NONE',  ( -18.05287651232776369, 33.35671069585768578, -57.55759232970981287 ) ) ;
#10972 = DIRECTION ( 'NONE',  ( -6.505213034913038160E-19, -3.903127820947822896E-18, -1.000000000000000000 ) ) ;
#10973 = CARTESIAN_POINT ( 'NONE',  ( 35.00000000000058265, 39.97500000000000142, -52.50000000000076739 ) ) ;
#10974 = EDGE_CURVE ( 'NONE', #6468, #10753, #15478, .T. ) ;
#10975 = CIRCLE ( 'NONE', #16840, 1.000000000000000888 ) ;
#10976 = VERTEX_POINT ( 'NONE', #10319 ) ;
#10977 = CYLINDRICAL_SURFACE ( 'NONE', #16368, 31.50000000000001421 ) ;
#10978 = DIRECTION ( 'NONE',  ( -0.000000000000000000, -1.000000000000000000, -0.000000000000000000 ) ) ;
#10979 = DIRECTION ( 'NONE',  ( 1.000000000000000000, 0.000000000000000000, 0.000000000000000000 ) ) ;
#10980 = CARTESIAN_POINT ( 'NONE',  ( 10.39230484541330846, -1.500000000000015099, -5.999999999999929834 ) ) ;
#10981 = DIRECTION ( 'NONE',  ( 0.000000000000000000, 1.000000000000000000, 0.000000000000000000 ) ) ;
#10982 = EDGE_LOOP ( 'NONE', ( #7369, #3037, #15035, #4454 ) ) ;
#10983 = DIRECTION ( 'NONE',  ( -6.505213034913038160E-19, -3.903127820947822896E-18, -1.000000000000000000 ) ) ;
#10984 = ORIENTED_EDGE ( 'NONE', *, *, #2899, .T. ) ;
#10985 = CYLINDRICAL_SURFACE ( 'NONE', #11142, 34.00000000000000000 ) ;
#10986 = DIRECTION ( 'NONE',  ( 1.000000000000000000, 0.000000000000000000, 0.000000000000000000 ) ) ;
#10987 = EDGE_CURVE ( 'NONE', #6067, #11258, #1639, .T. ) ;
#10988 = FACE_OUTER_BOUND ( 'NONE', #19901, .T. ) ;
#10989 = ORIENTED_EDGE ( 'NONE', *, *, #646, .F. ) ;
#10990 = DIRECTION ( 'NONE',  ( 1.000000000000000000, 0.000000000000000000, 0.000000000000000000 ) ) ;
#10991 = EDGE_CURVE ( 'NONE', #21584, #3760, #19167, .T. ) ;
#10992 = ORIENTED_EDGE ( 'NONE', *, *, #2501, .T. ) ;
#10993 = CARTESIAN_POINT ( 'NONE',  ( -4.104166344909047304, 35.92356703407487117, 2.932460736555809966 ) ) ;
#10994 = CARTESIAN_POINT ( 'NONE',  ( 25.00000000000000355, -20.00000000000000000, 16.49999999999999289 ) ) ;
#10995 = DIRECTION ( 'NONE',  ( 0.000000000000000000, -1.000000000000000000, 0.000000000000000000 ) ) ;
#10996 = VERTEX_POINT ( 'NONE', #14084 ) ;
#10997 = FACE_BOUND ( 'NONE', #13730, .T. ) ;
#10998 = EDGE_CURVE ( 'NONE', #7247, #12848, #17358, .T. ) ;
#10999 = DIRECTION ( 'NONE',  ( 0.000000000000000000, 0.000000000000000000, -1.000000000000000000 ) ) ;
#11000 = ORIENTED_EDGE ( 'NONE', *, *, #9050, .T. ) ;
#11001 = CARTESIAN_POINT ( 'NONE',  ( -21.69710536060276596, -28.14364593009914017, 3.000000000000058620 ) ) ;
#11002 = CARTESIAN_POINT ( 'NONE',  ( -17.32050807568873196, 1.500000000000015099, 9.999999999999772626 ) ) ;
#11003 = B_SPLINE_CURVE_WITH_KNOTS ( 'NONE', 3,
 ( #16725, #15330, #18559, #22006, #20610, #2873, #6413, #4924, #10177, #8026, #14987, #13380, #20399, #4709, #18679, #2983, #91, #5484, #13840, #21184, #7084, #325 ),
 .UNSPECIFIED., .F., .F.,
 ( 4, 2, 2, 2, 2, 2, 2, 2, 2, 2, 4 ),
 ( 0.007712149587921354570, 0.01231940472852628525, 0.01347121851367751207, 0.01462303229882873888, 0.01692665986913119078, 0.01807847365428241759, 0.01923028743943364788, 0.02153391500973611539, 0.02268572879488734567, 0.02383754258003857943, 0.02614117015034102959 ),
 .UNSPECIFIED. ) ;
#11004 = CARTESIAN_POINT ( 'NONE',  ( 18.83615802559801722, -32.14641817400232071, -6.999999999999950262 ) ) ;
#11005 = AXIS2_PLACEMENT_3D ( 'NONE', #4497, #9427, #1162 ) ;
#11006 = CARTESIAN_POINT ( 'NONE',  ( -15.49999999999980282, -2.516660498395516310, 60.00099999999999767 ) ) ;
#11007 = ADVANCED_FACE ( 'NONE', ( #12717 ), #5406, .T. ) ;
#11008 = ORIENTED_EDGE ( 'NONE', *, *, #13168, .F. ) ;
#11009 = DIRECTION ( 'NONE',  ( 6.505213034913038160E-19, 3.903127820947822896E-18, 1.000000000000000000 ) ) ;
#11010 = CARTESIAN_POINT ( 'NONE',  ( -12.84005703541686749, 1.693876179762715983, 55.76322220626266812 ) ) ;
#11011 = CARTESIAN_POINT ( 'NONE',  ( -3.944371625881058385, 39.90454848232354834, -51.54919429721285695 ) ) ;
#11012 = ORIENTED_EDGE ( 'NONE', *, *, #14399, .F. ) ;
#11013 = DIRECTION ( 'NONE',  ( -0.000000000000000000, 1.000000000000000000, -0.000000000000000000 ) ) ;
#11014 = DIRECTION ( 'NONE',  ( 0.000000000000000000, 0.000000000000000000, 1.000000000000000000 ) ) ;
#11016 = EDGE_CURVE ( 'NONE', #10179, #19351, #2662, .T. ) ;
#11015 = ORIENTED_EDGE ( 'NONE', *, *, #9598, .F. ) ;
#11017 = ORIENTED_EDGE ( 'NONE', *, *, #16463, .T. ) ;
#11018 = VERTEX_POINT ( 'NONE', #9627 ) ;
#11019 = EDGE_LOOP ( 'NONE', ( #8143, #2373, #20006, #9079 ) ) ;
#11020 = DIRECTION ( 'NONE',  ( -0.000000000000000000, -0.000000000000000000, 1.000000000000000000 ) ) ;
#11021 = DIRECTION ( 'NONE',  ( 0.000000000000000000, -1.000000000000000000, 0.000000000000000000 ) ) ;
#11022 = CARTESIAN_POINT ( 'NONE',  ( 35.00000000000000000, -4.999999999999997335, 4.258610482196280173E-15 ) ) ;
#11023 = ADVANCED_FACE ( 'NONE', ( #22125 ), #8142, .F. ) ;
#11024 = EDGE_LOOP ( 'NONE', ( #2767, #20545, #16513, #20118 ) ) ;
#11025 = CARTESIAN_POINT ( 'NONE',  ( -13.00000000000011546, 42.51666049839536043, 100.0000000000000000 ) ) ;
#11026 = CARTESIAN_POINT ( 'NONE',  ( -30.99230043872318063, 17.38334492574541557, -3.000000000000012879 ) ) ;
#11027 = ORIENTED_EDGE ( 'NONE', *, *, #5005, .T. ) ;
#11028 = CARTESIAN_POINT ( 'NONE',  ( 17.00000000000000000, 20.00000000000000711, -102.0000000000000142 ) ) ;
#11029 = CARTESIAN_POINT ( 'NONE',  ( -31.67162468655980589, -14.67611967928950101, 3.000000000000002665 ) ) ;
#11030 = AXIS2_PLACEMENT_3D ( 'NONE', #22399, #22294, #10448 ) ;
#11031 = CARTESIAN_POINT ( 'NONE',  ( -42.50000000000000711, -5.000000000000000000, -49.60000000000000142 ) ) ;
#11032 = ORIENTED_EDGE ( 'NONE', *, *, #4757, .F. ) ;
#11033 = DIRECTION ( 'NONE',  ( -0.000000000000000000, 1.000000000000000000, -0.000000000000000000 ) ) ;
#11034 = ORIENTED_EDGE ( 'NONE', *, *, #10630, .T. ) ;
#11035 = CARTESIAN_POINT ( 'NONE',  ( 3.244689583147291945, 39.74755540027157252, 52.34195286440930772 ) ) ;
#11036 = CARTESIAN_POINT ( 'NONE',  ( 0.6211727382237610673, 4.802676810931882923E-16, 50.97074642427956093 ) ) ;
#11037 = ORIENTED_EDGE ( 'NONE', *, *, #22659, .T. ) ;
#11038 = CARTESIAN_POINT ( 'NONE',  ( 16.66666666666669272, 20.00000000000000000, -23.57022603955159212 ) ) ;
#11039 = CARTESIAN_POINT ( 'NONE',  ( 9.870870746772787641, 37.43479630315659534, 54.49920060628448937 ) ) ;
#11040 = DIRECTION ( 'NONE',  ( 0.000000000000000000, 0.000000000000000000, 1.000000000000000000 ) ) ;
#11041 = CARTESIAN_POINT ( 'NONE',  ( 2.775557561562891351E-14, -2.775557561562891351E-14, 2.999999999999999112 ) ) ;
#11043 = EDGE_CURVE ( 'NONE', #19599, #10325, #4542, .T. ) ;
#11042 = VERTEX_POINT ( 'NONE', #6305 ) ;
#11044 = AXIS2_PLACEMENT_3D ( 'NONE', #165, #22541, #14130 ) ;
#11045 = ORIENTED_EDGE ( 'NONE', *, *, #7713, .T. ) ;
#11046 = VERTEX_POINT ( 'NONE', #9412 ) ;
#11047 = ORIENTED_EDGE ( 'NONE', *, *, #504, .T. ) ;
#11048 = DIRECTION ( 'NONE',  ( -0.000000000000000000, 1.000000000000000000, -0.000000000000000000 ) ) ;
#11049 = CYLINDRICAL_SURFACE ( 'NONE', #20250, 39.00000000000000000 ) ;
#11050 = CARTESIAN_POINT ( 'NONE',  ( 0.000000000000000000, 9.999999999999998224, 0.000000000000000000 ) ) ;
#11051 = EDGE_CURVE ( 'NONE', #1500, #16627, #8034, .T. ) ;
#11052 = ORIENTED_EDGE ( 'NONE', *, *, #9218, .F. ) ;
#11053 = DIRECTION ( 'NONE',  ( 1.000000000000000000, 0.000000000000000000, 0.000000000000000000 ) ) ;
#11054 = CARTESIAN_POINT ( 'NONE',  ( -4.084299015953898326, -4.682619376883251583, 48.27507093819014017 ) ) ;
#11055 = VERTEX_POINT ( 'NONE', #14772 ) ;
#11056 = DIRECTION ( 'NONE',  ( -6.505213034913038160E-19, -3.903127820947822896E-18, -1.000000000000000000 ) ) ;
#11057 = CARTESIAN_POINT ( 'NONE',  ( -34.99999999999999289, -5.000000000000000000, -3.012171160963566127E-14 ) ) ;
#11058 = DIRECTION ( 'NONE',  ( 6.505213034913038160E-19, 3.903127820947822896E-18, 1.000000000000000000 ) ) ;
#11059 = DIRECTION ( 'NONE',  ( 0.000000000000000000, 0.000000000000000000, 1.000000000000000000 ) ) ;
#11060 = ADVANCED_FACE ( 'NONE', ( #7688 ), #21787, .F. ) ;
#11061 = CIRCLE ( 'NONE', #22427, 34.00000000000000000 ) ;
#11062 = DIRECTION ( 'NONE',  ( 0.000000000000000000, 1.000000000000000000, 0.000000000000000000 ) ) ;
#11063 = DIRECTION ( 'NONE',  ( 0.000000000000000000, -1.000000000000000000, 0.000000000000000000 ) ) ;
#11064 = EDGE_CURVE ( 'NONE', #9114, #11241, #13387, .T. ) ;
#11065 = CARTESIAN_POINT ( 'NONE',  ( -0.6290164960542528050, 40.00000000000000000, 49.48738346576863023 ) ) ;
#11066 = DIRECTION ( 'NONE',  ( 1.000000000000000000, 0.000000000000000000, 0.000000000000000000 ) ) ;
#11067 = VERTEX_POINT ( 'NONE', #2424 ) ;
#11068 = ORIENTED_EDGE ( 'NONE', *, *, #21533, .T. ) ;
#11069 = ORIENTED_EDGE ( 'NONE', *, *, #14871, .T. ) ;
#11070 = CIRCLE ( 'NONE', #7773, 0.9999999999999974465 ) ;
#11071 = DIRECTION ( 'NONE',  ( -0.000000000000000000, -1.000000000000000000, -0.000000000000000000 ) ) ;
#11072 = DIRECTION ( 'NONE',  ( 1.000000000000000000, 1.208970125616053321E-17, 0.000000000000000000 ) ) ;
#11073 = CARTESIAN_POINT ( 'NONE',  ( 6.002321937223278780, -0.8366808808176150469, -52.11647083208271169 ) ) ;
#11074 = AXIS2_PLACEMENT_3D ( 'NONE', #4296, #14591, #5544 ) ;
#11075 = CARTESIAN_POINT ( 'NONE',  ( 31.92986134326233838, -18.22261011550285659, -1.999999999999998224 ) ) ;
#11076 = CARTESIAN_POINT ( 'NONE',  ( 5.233625953339160397E-15, -0.1272971988267498356, 49.60954963577236043 ) ) ;
#11077 = LINE ( 'NONE', #19464, #18608 ) ;
#11078 = CARTESIAN_POINT ( 'NONE',  ( -1.268121568161834523, 39.97056933375375110, -50.22305475357490678 ) ) ;
#11079 = DIRECTION ( 'NONE',  ( 6.505213034913038160E-19, 3.903127820947822896E-18, 1.000000000000000000 ) ) ;
#11080 = DIRECTION ( 'NONE',  ( 1.296372316667914327E-16, 1.000000000000000000, -0.000000000000000000 ) ) ;
#11081 = VERTEX_POINT ( 'NONE', #11462 ) ;
#11082 = CARTESIAN_POINT ( 'NONE',  ( -42.50000000000000711, -5.000000000000000000, 47.50000000000000711 ) ) ;
#11083 = DIRECTION ( 'NONE',  ( -0.000000000000000000, 1.000000000000000000, -0.000000000000000000 ) ) ;
#11084 = DIRECTION ( 'NONE',  ( 0.000000000000000000, -1.000000000000000000, 0.000000000000000000 ) ) ;
#11085 = FACE_OUTER_BOUND ( 'NONE', #19326, .T. ) ;
#11086 = DIRECTION ( 'NONE',  ( -6.505213034913038160E-19, -3.903127820947822896E-18, -1.000000000000000000 ) ) ;
#11087 = ADVANCED_FACE ( 'NONE', ( #18450 ), #13047, .F. ) ;
#11088 = VERTEX_POINT ( 'NONE', #11579 ) ;
#11089 = CIRCLE ( 'NONE', #4152, 6.499999999999999112 ) ;
#11090 = VERTEX_POINT ( 'NONE', #18568 ) ;
#11091 = DIRECTION ( 'NONE',  ( -6.505213034913038160E-19, -3.903127820947822896E-18, -1.000000000000000000 ) ) ;
#11092 = CARTESIAN_POINT ( 'NONE',  ( -34.99999999999999289, -5.000000000000000000, -52.49999999999705125 ) ) ;
#11093 = CIRCLE ( 'NONE', #9638, 10.00000000000000178 ) ;
#11094 = TOROIDAL_SURFACE ( 'NONE', #3058, 50.00000000000000000, 10.00000000000000000 ) ;
#11095 = ORIENTED_EDGE ( 'NONE', *, *, #933, .T. ) ;
#11096 = CARTESIAN_POINT ( 'NONE',  ( 34.10919265018095103, -11.98978967046217825, 2.932969818539045370 ) ) ;
#11097 = EDGE_CURVE ( 'NONE', #10123, #15736, #17690, .T. ) ;
#11098 = TOROIDAL_SURFACE ( 'NONE', #9634, 22.00000000000000000, 2.000000000000000000 ) ;
#11099 = CARTESIAN_POINT ( 'NONE',  ( 7.725164357189188813, 40.00000000000000000, -52.85294098179745248 ) ) ;
#11100 = EDGE_LOOP ( 'NONE', ( #9928, #10134, #19004, #12845 ) ) ;
#11101 = CARTESIAN_POINT ( 'NONE',  ( 4.586071060776173880, 39.86904401650008367, -51.95542086194134157 ) ) ;
#11102 = CARTESIAN_POINT ( 'NONE',  ( 23.49999999999998579, 19.99999999999999645, -100.0000000000000000 ) ) ;
#11103 = AXIS2_PLACEMENT_3D ( 'NONE', #11050, #17821, #2130 ) ;
#11104 = CARTESIAN_POINT ( 'NONE',  ( 4.724946350300523916E-15, 8.251288694035745053, 0.000000000000000000 ) ) ;
#11105 = ORIENTED_EDGE ( 'NONE', *, *, #1725, .F. ) ;
#11106 = CARTESIAN_POINT ( 'NONE',  ( 35.00000000000058265, 28.00000000000000000, -57.50000000000076028 ) ) ;
#11107 = AXIS2_PLACEMENT_3D ( 'NONE', #9862, #16851, #6083 ) ;
#11108 = CARTESIAN_POINT ( 'NONE',  ( -9.750125222798885716, 39.99999999999999289, 53.58569999979536647 ) ) ;
#11109 = ORIENTED_EDGE ( 'NONE', *, *, #9270, .T. ) ;
#11110 = ADVANCED_FACE ( 'NONE', ( #2652 ), #2709, .F. ) ;
#11112 = EDGE_CURVE ( 'NONE', #21024, #5921, #18790, .T. ) ;
#11111 = DIRECTION ( 'NONE',  ( 0.000000000000000000, 0.000000000000000000, 1.000000000000000000 ) ) ;
#11113 = AXIS2_PLACEMENT_3D ( 'NONE', #560, #8926, #2399 ) ;
#11114 = CARTESIAN_POINT ( 'NONE',  ( -7.549837901776227156, 39.99999999999999289, 52.78128042259339736 ) ) ;
#11115 = CYLINDRICAL_SURFACE ( 'NONE', #21307, 5.000000000000000000 ) ;
#11116 = ORIENTED_EDGE ( 'NONE', *, *, #10432, .F. ) ;
#11117 = CARTESIAN_POINT ( 'NONE',  ( 3.330669073875469621E-13, -1.110223024625156540E-13, -2.999999999999971578 ) ) ;
#11118 = CARTESIAN_POINT ( 'NONE',  ( -1.011722470947959973, -35.51751788033354984, -2.999999999999999112 ) ) ;
#11119 = CARTESIAN_POINT ( 'NONE',  ( -2.239819223192103692, 39.96978031709322465, -50.39586371513333063 ) ) ;
#11120 = EDGE_LOOP ( 'NONE', ( #8280, #4359, #6183, #8131 ) ) ;
#11121 = DIRECTION ( 'NONE',  ( -0.000000000000000000, 1.000000000000000000, -0.000000000000000000 ) ) ;
#11122 = TOROIDAL_SURFACE ( 'NONE', #15870, 34.90673715956759082, 8.750000000000000000 ) ;
#11123 = AXIS2_PLACEMENT_3D ( 'NONE', #7458, #2423, #16390 ) ;
#11124 = VERTEX_POINT ( 'NONE', #19948 ) ;
#11125 = VERTEX_POINT ( 'NONE', #11229 ) ;
#11126 = EDGE_CURVE ( 'NONE', #19011, #18643, #4891, .T. ) ;
#11127 = ORIENTED_EDGE ( 'NONE', *, *, #9996, .T. ) ;
#11128 = VERTEX_POINT ( 'NONE', #16950 ) ;
#11129 = FACE_OUTER_BOUND ( 'NONE', #19542, .T. ) ;
#11130 = CARTESIAN_POINT ( 'NONE',  ( 7.899727005596350438, 39.58366633022075121, -53.79762619906099275 ) ) ;
#11131 = LINE ( 'NONE', #20084, #16006 ) ;
#11132 = AXIS2_PLACEMENT_3D ( 'NONE', #8730, #8611, #19391 ) ;
#11133 = DIRECTION ( 'NONE',  ( -1.000000000000000000, 0.000000000000000000, 0.000000000000000000 ) ) ;
#11134 = EDGE_LOOP ( 'NONE', ( #12502, #7047, #14066, #9878, #7159, #4884 ) ) ;
#11135 = DIRECTION ( 'NONE',  ( 6.505213034913038160E-19, 3.903127820947822896E-18, 1.000000000000000000 ) ) ;
#11136 = DIRECTION ( 'NONE',  ( 1.296372316667914327E-16, 1.000000000000000000, -0.000000000000000000 ) ) ;
#11137 = ORIENTED_EDGE ( 'NONE', *, *, #19365, .F. ) ;
#11138 = EDGE_CURVE ( 'NONE', #2407, #6416, #17953, .T. ) ;
#11139 = ADVANCED_FACE ( 'NONE', ( #22587 ), #7448, .F. ) ;
#11140 = LINE ( 'NONE', #3719, #7583 ) ;
#11141 = CYLINDRICAL_SURFACE ( 'NONE', #955, 31.50000000000000711 ) ;
#11142 = AXIS2_PLACEMENT_3D ( 'NONE', #7551, #4354, #5941 ) ;
#11143 = CYLINDRICAL_SURFACE ( 'NONE', #3875, 6.499999999999999112 ) ;
#11144 = ORIENTED_EDGE ( 'NONE', *, *, #4527, .F. ) ;
#11145 = CARTESIAN_POINT ( 'NONE',  ( 35.00000000000000000, 17.00000000000000000, 41.00000000000002132 ) ) ;
#11146 = DIRECTION ( 'NONE',  ( -1.224646799147353207E-16, 0.000000000000000000, 1.000000000000000000 ) ) ;
#11147 = ORIENTED_EDGE ( 'NONE', *, *, #10291, .F. ) ;
#11148 = CARTESIAN_POINT ( 'NONE',  ( 4.278324951947499954, 39.54020021135884377, 53.33400390260334945 ) ) ;
#11149 = DIRECTION ( 'NONE',  ( 0.000000000000000000, 1.000000000000000000, -0.000000000000000000 ) ) ;
#11150 = VERTEX_POINT ( 'NONE', #2990 ) ;
#11151 = DIRECTION ( 'NONE',  ( 0.000000000000000000, 0.000000000000000000, 1.000000000000000000 ) ) ;
#11152 = FACE_OUTER_BOUND ( 'NONE', #2638, .T. ) ;
#11153 = ADVANCED_FACE ( 'NONE', ( #1490 ), #20275, .T. ) ;
#11154 = CARTESIAN_POINT ( 'NONE',  ( 35.00000000000058265, 40.00000000000000711, -55.00000000000076028 ) ) ;
#11155 = CARTESIAN_POINT ( 'NONE',  ( -22.28024240313504478, -22.26748298433264850, -2.999999999999999112 ) ) ;
#11156 = AXIS2_PLACEMENT_3D ( 'NONE', #9841, #11768, #22102 ) ;
#11157 = ORIENTED_EDGE ( 'NONE', *, *, #15425, .F. ) ;
#11158 = ORIENTED_EDGE ( 'NONE', *, *, #1810, .T. ) ;
#11159 = ORIENTED_EDGE ( 'NONE', *, *, #4435, .T. ) ;
#11160 = ORIENTED_EDGE ( 'NONE', *, *, #520, .F. ) ;
#11161 = DIRECTION ( 'NONE',  ( 0.000000000000000000, 0.000000000000000000, 1.000000000000000000 ) ) ;
#11162 = DIRECTION ( 'NONE',  ( 0.000000000000000000, 0.000000000000000000, -1.000000000000000000 ) ) ;
#11163 = EDGE_CURVE ( 'NONE', #13942, #12412, #3479, .T. ) ;
#11164 = CYLINDRICAL_SURFACE ( 'NONE', #12552, 25.00000000000000000 ) ;
#11165 = EDGE_LOOP ( 'NONE', ( #2104, #19928, #7479, #1165 ) ) ;
#11166 = CARTESIAN_POINT ( 'NONE',  ( -1.387778780781445676E-14, 20.00000000000000000, -98.00000000000000000 ) ) ;
#11167 = CIRCLE ( 'NONE', #15539, 39.00000000000000000 ) ;
#11168 = VECTOR ( 'NONE', #6638, 1000.000000000000000 ) ;
#11169 = ORIENTED_EDGE ( 'NONE', *, *, #4547, .F. ) ;
#11170 = DIRECTION ( 'NONE',  ( -1.000000000000000000, -1.208970125616044077E-17, 0.000000000000000000 ) ) ;
#11171 = CARTESIAN_POINT ( 'NONE',  ( 2.999999999999998224, 22.00000000000000000, 8.485281374238567764 ) ) ;
#11172 = DIRECTION ( 'NONE',  ( 0.000000000000000000, 0.000000000000000000, 1.000000000000000000 ) ) ;
#11173 = ADVANCED_FACE ( 'NONE', ( #12031 ), #6718, .T. ) ;
#11174 = VECTOR ( 'NONE', #18534, 1000.000000000000000 ) ;
#11175 = EDGE_CURVE ( 'NONE', #19744, #22334, #500, .T. ) ;
#11176 = CARTESIAN_POINT ( 'NONE',  ( 27.56232195404084706, -21.41958700883264655, -2.999999999999954259 ) ) ;
#11177 = CARTESIAN_POINT ( 'NONE',  ( 5.833333333333437842, 6.180730040185884455, -40.61164310337073857 ) ) ;
#11178 = DIRECTION ( 'NONE',  ( -4.718764931986839378E-35, 3.903127820947822896E-18, 1.000000000000000000 ) ) ;
#11179 = ADVANCED_FACE ( 'NONE', ( #20860 ), #18910, .F. ) ;
#11180 = CARTESIAN_POINT ( 'NONE',  ( -22.97438720605733664, 22.98755168577407204, -2.999999999999971578 ) ) ;
#11181 = VECTOR ( 'NONE', #18688, 1000.000000000000000 ) ;
#11182 = EDGE_LOOP ( 'NONE', ( #6710, #4979, #4937, #11032 ) ) ;
#11183 = ORIENTED_EDGE ( 'NONE', *, *, #21500, .T. ) ;
#11184 = VECTOR ( 'NONE', #12574, 1000.000000000000000 ) ;
#11185 = ORIENTED_EDGE ( 'NONE', *, *, #8892, .F. ) ;
#11186 = AXIS2_PLACEMENT_3D ( 'NONE', #20386, #16367, #6514 ) ;
#11187 = DIRECTION ( 'NONE',  ( 0.000000000000000000, 1.000000000000000000, 0.000000000000000000 ) ) ;
#11188 = CARTESIAN_POINT ( 'NONE',  ( -0.6212853642548137323, -1.852178711329401354E-16, -50.97083105892616572 ) ) ;
#11189 = EDGE_CURVE ( 'NONE', #4971, #2350, #5976, .T. ) ;
#11190 = CARTESIAN_POINT ( 'NONE',  ( 4.240553750831081103, 39.54840718952534218, 53.29860200223214406 ) ) ;
#11191 = DIRECTION ( 'NONE',  ( 0.000000000000000000, 0.000000000000000000, -1.000000000000000000 ) ) ;
#11192 = VECTOR ( 'NONE', #12451, 1000.000000000000000 ) ;
#11193 = FACE_OUTER_BOUND ( 'NONE', #15583, .T. ) ;
#11194 = CARTESIAN_POINT ( 'NONE',  ( 3.330669073875469621E-13, -1.110223024625156540E-13, -2.999999999999971578 ) ) ;
#11195 = CYLINDRICAL_SURFACE ( 'NONE', #14944, 2.499999999999998668 ) ;
#11196 = CARTESIAN_POINT ( 'NONE',  ( 14.30873905802362778, 28.06260833510296138, 2.999999999999995559 ) ) ;
#11197 = CIRCLE ( 'NONE', #20731, 15.00000000000000000 ) ;
#11198 = EDGE_LOOP ( 'NONE', ( #14615, #18036, #6422, #11518 ) ) ;
#11199 = DIRECTION ( 'NONE',  ( 0.000000000000000000, 0.000000000000000000, 1.000000000000000000 ) ) ;
#11200 = DIRECTION ( 'NONE',  ( 0.000000000000000000, 0.000000000000000000, -1.000000000000000000 ) ) ;
#11201 = DIRECTION ( 'NONE',  ( 0.000000000000000000, 0.000000000000000000, 1.000000000000000000 ) ) ;
#11202 = FACE_OUTER_BOUND ( 'NONE', #17330, .T. ) ;
#11203 = CYLINDRICAL_SURFACE ( 'NONE', #14015, 2.099999999999997868 ) ;
#11204 = CIRCLE ( 'NONE', #11586, 1.000000000000000888 ) ;
#11205 = EDGE_LOOP ( 'NONE', ( #15523, #17104, #17722, #20020, #1529, #9568 ) ) ;
#11206 = ORIENTED_EDGE ( 'NONE', *, *, #19592, .T. ) ;
#11207 = DIRECTION ( 'NONE',  ( -0.000000000000000000, -1.000000000000000000, -0.000000000000000000 ) ) ;
#11208 = DIRECTION ( 'NONE',  ( -1.000000000000000000, 0.000000000000000000, 0.000000000000000000 ) ) ;
#11209 = ORIENTED_EDGE ( 'NONE', *, *, #14998, .F. ) ;
#11210 = CIRCLE ( 'NONE', #4661, 2.525000000000110489 ) ;
#11211 = EDGE_CURVE ( 'NONE', #3042, #121, #15844, .T. ) ;
#11212 = LINE ( 'NONE', #16601, #12945 ) ;
#11213 = CYLINDRICAL_SURFACE ( 'NONE', #20028, 3.999999999999998224 ) ;
#11214 = ORIENTED_EDGE ( 'NONE', *, *, #16902, .F. ) ;
#11215 = CARTESIAN_POINT ( 'NONE',  ( 0.4444706617113970970, 39.99884075969093544, -49.07683524994765634 ) ) ;
#11216 = VECTOR ( 'NONE', #20019, 1000.000000000000114 ) ;
#11217 = CARTESIAN_POINT ( 'NONE',  ( -17.86915608785671949, 27.01645732367855146, 2.999999999999995559 ) ) ;
#11218 = VERTEX_POINT ( 'NONE', #1600 ) ;
#11219 = DIRECTION ( 'NONE',  ( -1.000000000000000000, -1.208970125616060101E-17, 6.505213034913038160E-19 ) ) ;
#11220 = FACE_OUTER_BOUND ( 'NONE', #12641, .T. ) ;
#11221 = ORIENTED_EDGE ( 'NONE', *, *, #10691, .T. ) ;
#11222 = CARTESIAN_POINT ( 'NONE',  ( -13.56354382738803466, 2.142135623730933247, -56.03997097393685323 ) ) ;
#11223 = CARTESIAN_POINT ( 'NONE',  ( 13.31210290807009322, 38.06413856043591437, -55.94798518138998844 ) ) ;
#11224 = DIRECTION ( 'NONE',  ( -0.000000000000000000, -1.000000000000000000, -0.000000000000000000 ) ) ;
#11225 = ORIENTED_EDGE ( 'NONE', *, *, #9723, .T. ) ;
#11226 = DIRECTION ( 'NONE',  ( -6.505213034913038160E-19, -3.903127820947822896E-18, -1.000000000000000000 ) ) ;
#11227 = AXIS2_PLACEMENT_3D ( 'NONE', #7942, #21930, #15017 ) ;
#11228 = FACE_BOUND ( 'NONE', #15344, .T. ) ;
#11229 = CARTESIAN_POINT ( 'NONE',  ( 12.00937115242667375, 34.74700806321082069, -2.800654218530485018 ) ) ;
#11230 = CIRCLE ( 'NONE', #19317, 2.524999999999999467 ) ;
#11231 = ORIENTED_EDGE ( 'NONE', *, *, #14388, .T. ) ;
#11232 = DIRECTION ( 'NONE',  ( -1.000000000000000000, 1.301042606982605814E-16, 0.000000000000000000 ) ) ;
#11233 = EDGE_CURVE ( 'NONE', #2030, #2015, #5272, .T. ) ;
#11234 = CARTESIAN_POINT ( 'NONE',  ( -11.93972437435557232, -29.14949368109881433, 3.000000000000023537 ) ) ;
#11235 = CARTESIAN_POINT ( 'NONE',  ( 13.00000000000000178, 20.00000000000000000, -11.32475165290605901 ) ) ;
#11236 = ADVANCED_FACE ( 'NONE', ( #1078 ), #17178, .F. ) ;
#11237 = ORIENTED_EDGE ( 'NONE', *, *, #5832, .F. ) ;
#11238 = CIRCLE ( 'NONE', #1366, 1.000000000000000888 ) ;
#11239 = ORIENTED_EDGE ( 'NONE', *, *, #15883, .T. ) ;
#11240 = VECTOR ( 'NONE', #4475, 1000.000000000000000 ) ;
#11241 = VERTEX_POINT ( 'NONE', #17064 ) ;
#11242 = DIRECTION ( 'NONE',  ( 0.2124049323636610365, -0.9771811438690338747, -0.001075534469410268637 ) ) ;
#11243 = UNCERTAINTY_MEASURE_WITH_UNIT (LENGTH_MEASURE( 1.000000000000000082E-05 ), #17257, 'distance_accuracy_value', 'NONE');
#11244 = VECTOR ( 'NONE', #6041, 1000.000000000000000 ) ;
#11245 = ORIENTED_EDGE ( 'NONE', *, *, #5518, .T. ) ;
#11246 = CARTESIAN_POINT ( 'NONE',  ( 19.71583072461104535, 23.39500837205462602, -60.55395521980172902 ) ) ;
#11247 = CARTESIAN_POINT ( 'NONE',  ( 8.523345606421392162, -2.856915207551451452, 52.89411661606261106 ) ) ;
#11248 = DIRECTION ( 'NONE',  ( 0.000000000000000000, -0.7071067811867928210, -0.7071067811863022134 ) ) ;
#11249 = CARTESIAN_POINT ( 'NONE',  ( -17.00000000000000000, 20.00000000000000711, 102.0000000000000142 ) ) ;
#11250 = CARTESIAN_POINT ( 'NONE',  ( 3.469446951953614189E-15, 38.23275711891355400, 0.000000000000000000 ) ) ;
#11251 = ORIENTED_EDGE ( 'NONE', *, *, #16707, .T. ) ;
#11252 = CARTESIAN_POINT ( 'NONE',  ( 1.110223024625156540E-13, -5.551115123125782702E-14, -6.999999999999950262 ) ) ;
#11253 = CARTESIAN_POINT ( 'NONE',  ( -10.00000000000000000, -4.824555320336763486, -3.000000000000000000 ) ) ;
#11254 = ORIENTED_EDGE ( 'NONE', *, *, #19789, .F. ) ;
#11255 = CARTESIAN_POINT ( 'NONE',  ( -35.00000000000000000, 15.00000000000000000, 41.00000000000002132 ) ) ;
#11256 = CARTESIAN_POINT ( 'NONE',  ( -16.26546936781298314, 4.421830200407484313, -57.01255691153426852 ) ) ;
#11257 = CARTESIAN_POINT ( 'NONE',  ( 19.52068517772377376, 15.62943592677015126, -60.50640500721814163 ) ) ;
#11258 = VERTEX_POINT ( 'NONE', #1372 ) ;
#11259 = CARTESIAN_POINT ( 'NONE',  ( 33.51030287062386748, 15.12081897056644131, -1.999999999999970468 ) ) ;
#11260 = FACE_OUTER_BOUND ( 'NONE', #16131, .T. ) ;
#11261 = CONICAL_SURFACE ( 'NONE', #1381, 58.99999999999698730, 0.7853981633974447263 ) ;
#11262 = VERTEX_POINT ( 'NONE', #8586 ) ;
#11263 = CARTESIAN_POINT ( 'NONE',  ( 6.433485051969655366, 38.94088993357593154, 55.16018527340020938 ) ) ;
#11264 = CARTESIAN_POINT ( 'NONE',  ( -1.485717122675851432, -1.299971956346734459, 49.29290837556845872 ) ) ;
#11265 = EDGE_LOOP ( 'NONE', ( #4960, #910, #7460, #13719 ) ) ;
#11266 = AXIS2_PLACEMENT_3D ( 'NONE', #17167, #4921, #1589 ) ;
#11267 = EDGE_CURVE ( 'NONE', #3791, #478, #8902, .T. ) ;
#11268 = AXIS2_PLACEMENT_3D ( 'NONE', #20010, #9575, #13444 ) ;
#11269 = DIRECTION ( 'NONE',  ( 0.000000000000000000, -1.000000000000000000, 0.000000000000000000 ) ) ;
#11270 = DIRECTION ( 'NONE',  ( -0.000000000000000000, -1.000000000000000000, -0.000000000000000000 ) ) ;
#11271 = AXIS2_PLACEMENT_3D ( 'NONE', #11648, #3178, #20479 ) ;
#11272 = FACE_OUTER_BOUND ( 'NONE', #6159, .T. ) ;
#11273 = EDGE_CURVE ( 'NONE', #2292, #4146, #6193, .T. ) ;
#11274 = EDGE_CURVE ( 'NONE', #1434, #4151, #11830, .T. ) ;
#11275 = VERTEX_POINT ( 'NONE', #13844 ) ;
#11276 = ORIENTED_EDGE ( 'NONE', *, *, #9484, .T. ) ;
#11277 = CIRCLE ( 'NONE', #16024, 18.00000000000000355 ) ;
#11278 = ORIENTED_EDGE ( 'NONE', *, *, #9270, .F. ) ;
#11279 = ORIENTED_EDGE ( 'NONE', *, *, #16812, .T. ) ;
#11280 = DIRECTION ( 'NONE',  ( -6.505213034913038160E-19, -3.903127820947822896E-18, -1.000000000000000000 ) ) ;
#11281 = AXIS2_PLACEMENT_3D ( 'NONE', #3380, #15728, #10338 ) ;
#11282 = CARTESIAN_POINT ( 'NONE',  ( 35.00000000000000000, 40.00000000000000000, 4.258610482196280173E-15 ) ) ;
#11283 = CONICAL_SURFACE ( 'NONE', #17495, 2.099999999999997868, 1.029744258676653867 ) ;
#11284 = CARTESIAN_POINT ( 'NONE',  ( -27.64365646977254443, -17.09029715894946833, 3.000000000000012879 ) ) ;
#11285 = EDGE_CURVE ( 'NONE', #11348, #2120, #5164, .T. ) ;
#11286 = VERTEX_POINT ( 'NONE', #10403 ) ;
#11287 = DIRECTION ( 'NONE',  ( 0.000000000000000000, 0.000000000000000000, 1.000000000000000000 ) ) ;
#11288 = CARTESIAN_POINT ( 'NONE',  ( 0.005803611680460589971, 39.99999985006627412, 48.73848948830625716 ) ) ;
#11289 = ORIENTED_EDGE ( 'NONE', *, *, #3684, .F. ) ;
#11290 = ORIENTED_EDGE ( 'NONE', *, *, #21092, .T. ) ;
#11291 = CARTESIAN_POINT ( 'NONE',  ( -17.38334492574528767, -30.99230043872344709, -2.999999999999998224 ) ) ;
#11292 = ADVANCED_FACE ( 'NONE', ( #2274 ), #18058, .F. ) ;
#11293 = DIRECTION ( 'NONE',  ( 0.000000000000000000, -1.000000000000000000, 0.000000000000000000 ) ) ;
#11294 = DIRECTION ( 'NONE',  ( -0.000000000000000000, -1.000000000000000000, -0.000000000000000000 ) ) ;
#11295 = SURFACE_SIDE_STYLE ('',( #9231 ) ) ;
#11296 = EDGE_CURVE ( 'NONE', #5732, #5053, #14747, .T. ) ;
#11297 = VECTOR ( 'NONE', #11653, 999.9999999999998863 ) ;
#11298 = CIRCLE ( 'NONE', #5447, 0.9999999999999991118 ) ;
#11299 = DIRECTION ( 'NONE',  ( -6.505213034913038160E-19, -3.903127820947822896E-18, -1.000000000000000000 ) ) ;
#11300 = DIRECTION ( 'NONE',  ( -1.000000000000000000, 0.000000000000000000, 0.000000000000000000 ) ) ;
#11301 = DIRECTION ( 'NONE',  ( 0.000000000000000000, 0.000000000000000000, -1.000000000000000000 ) ) ;
#11302 = AXIS2_PLACEMENT_3D ( 'NONE', #16515, #14891, #19851 ) ;
#11303 = EDGE_LOOP ( 'NONE', ( #6141, #21372, #15426, #830, #6457 ) ) ;
#11304 = EDGE_CURVE ( 'NONE', #22506, #675, #11093, .T. ) ;
#11305 = ORIENTED_EDGE ( 'NONE', *, *, #20514, .F. ) ;
#11306 = ADVANCED_FACE ( 'NONE', ( #9260 ), #14003, .F. ) ;
#11307 = VERTEX_POINT ( 'NONE', #17970 ) ;
#11308 = CARTESIAN_POINT ( 'NONE',  ( -18.99835506941826679, 13.52193747355387821, 57.87905887291319829 ) ) ;
#11309 = LINE ( 'NONE', #4211, #7099 ) ;
#11310 = EDGE_CURVE ( 'NONE', #22272, #4064, #20617, .T. ) ;
#11311 = AXIS2_PLACEMENT_3D ( 'NONE', #2486, #3862, #10828 ) ;
#11312 = CIRCLE ( 'NONE', #17159, 2.499999999999995115 ) ;
#11313 = DIRECTION ( 'NONE',  ( 0.000000000000000000, -0.7071067811865500152, -0.7071067811865451302 ) ) ;
#11314 = CARTESIAN_POINT ( 'NONE',  ( -1.045703040280289819, 0.02735608008923263654, -49.70561346074465803 ) ) ;
#11315 = ADVANCED_FACE ( 'NONE', ( #17741, #16243 ), #10519, .F. ) ;
#11316 = CARTESIAN_POINT ( 'NONE',  ( 11.68090480754630178, 3.765577839755386069, 57.90797000640142045 ) ) ;
#11317 = DIRECTION ( 'NONE',  ( -0.000000000000000000, -1.000000000000000000, -0.000000000000000000 ) ) ;
#11318 = DIRECTION ( 'NONE',  ( -1.000000000000000000, 0.000000000000000000, 0.000000000000000000 ) ) ;
#11319 = DIRECTION ( 'NONE',  ( 0.000000000000000000, 0.7071067811865451302, 0.7071067811865500152 ) ) ;
#11320 = FACE_OUTER_BOUND ( 'NONE', #10609, .T. ) ;
#11321 = VERTEX_POINT ( 'NONE', #3560 ) ;
#11322 = CARTESIAN_POINT ( 'NONE',  ( 2.602085213965210642E-15, 7.999999999999994671, 19.00000000000000355 ) ) ;
#11323 = B_SPLINE_CURVE_WITH_KNOTS ( 'NONE', 3,
 ( #11591, #6435, #18586, #16518, #22024, #1055, #20082, #13277, #9759, #6316, #2775, #18244, #6212, #8047, #4732, #13398, #1159, #19962, #11246, #5981, #18125, #15006 ),
 .UNSPECIFIED., .F., .F.,
 ( 4, 2, 2, 2, 2, 2, 2, 2, 2, 2, 4 ),
 ( 0.000000000000000000, 0.005822207826702249442, 0.007277759783377814838, 0.008733311740053378500, 0.01164441565340452144, 0.01309996761008009811, 0.01455551956675567304, 0.01746662348010682639, 0.01892217543678240479, 0.02037772739345798320, 0.02328883130680912614 ),
 .UNSPECIFIED. ) ;
#11324 = DIRECTION ( 'NONE',  ( 0.000000000000000000, 0.000000000000000000, -1.000000000000000000 ) ) ;
#11325 = CARTESIAN_POINT ( 'NONE',  ( -24.41514043009178181, -26.50842683089757301, -6.999999999999999112 ) ) ;
#11326 = CARTESIAN_POINT ( 'NONE',  ( -6.000000000000000000, -20.00000000000000000, -5.999999999999999112 ) ) ;
#11327 = CARTESIAN_POINT ( 'NONE',  ( 6.070730550690961458, 31.88709182564675260, -6.999999999999950262 ) ) ;
#11328 = ORIENTED_EDGE ( 'NONE', *, *, #6804, .F. ) ;
#11329 = FACE_BOUND ( 'NONE', #21016, .T. ) ;
#11330 = EDGE_LOOP ( 'NONE', ( #9394, #1061, #16025 ) ) ;
#11331 = CIRCLE ( 'NONE', #4017, 16.49999999999998579 ) ;
#11332 = DIRECTION ( 'NONE',  ( 1.000000000000000000, 0.000000000000000000, 0.000000000000000000 ) ) ;
#11333 = DIRECTION ( 'NONE',  ( 0.000000000000000000, 1.000000000000000000, 0.000000000000000000 ) ) ;
#11334 = ORIENTED_EDGE ( 'NONE', *, *, #17148, .T. ) ;
#11335 = EDGE_CURVE ( 'NONE', #19717, #950, #14383, .T. ) ;
#11336 = DIRECTION ( 'NONE',  ( -0.000000000000000000, 1.000000000000000000, -0.000000000000000000 ) ) ;
#11337 = AXIS2_PLACEMENT_3D ( 'NONE', #15458, #10082, #15696 ) ;
#11338 = CARTESIAN_POINT ( 'NONE',  ( 6.176815998947249753, 40.00000000000000000, -52.17714723720779801 ) ) ;
#11339 = ORIENTED_EDGE ( 'NONE', *, *, #22505, .F. ) ;
#11340 = CARTESIAN_POINT ( 'NONE',  ( 0.9695974223849092022, 39.99443194917778754, -49.47365400635877108 ) ) ;
#11341 = CARTESIAN_POINT ( 'NONE',  ( 35.00000000000001421, 0.000000000000000000, 1.540743955509788682E-30 ) ) ;
#11342 =( GEOMETRIC_REPRESENTATION_CONTEXT ( 3 ) GLOBAL_UNCERTAINTY_ASSIGNED_CONTEXT ( ( #4407 ) ) GLOBAL_UNIT_ASSIGNED_CONTEXT ( ( #180, #20943, #15764 ) ) REPRESENTATION_CONTEXT ( 'NONE', 'WORKASPACE' ) );
#11343 = CARTESIAN_POINT ( 'NONE',  ( 5.833333333333329485, 39.00000000000000711, -40.61164310337066041 ) ) ;
#11344 = CARTESIAN_POINT ( 'NONE',  ( -6.000000000000000000, 20.00000000000000000, -5.999999999999999112 ) ) ;
#11345 = CARTESIAN_POINT ( 'NONE',  ( 23.49999999999998579, 19.99999999999999645, 60.00099999999999767 ) ) ;
#11346 = CARTESIAN_POINT ( 'NONE',  ( -1.571417673354765121, 40.00000000000000711, 49.72695664780195557 ) ) ;
#11347 = DIRECTION ( 'NONE',  ( -0.000000000000000000, -1.000000000000000000, -0.000000000000000000 ) ) ;
#11348 = VERTEX_POINT ( 'NONE', #14174 ) ;
#11349 = CARTESIAN_POINT ( 'NONE',  ( 6.955395936297148474, 34.84717828836173226, -3.000000000000006217 ) ) ;
#11350 = DIRECTION ( 'NONE',  ( -4.718764931986839378E-35, 3.903127820947822896E-18, 1.000000000000000000 ) ) ;
#11351 = CARTESIAN_POINT ( 'NONE',  ( -0.03961255302991764649, 39.99999109211487536, -48.76478634770423071 ) ) ;
#11352 = EDGE_CURVE ( 'NONE', #407, #8973, #19708, .T. ) ;
#11353 = VERTEX_POINT ( 'NONE', #1835 ) ;
#11354 = CIRCLE ( 'NONE', #19430, 3.000000000000000888 ) ;
#11355 = CARTESIAN_POINT ( 'NONE',  ( -13.25963002225074128, 27.02330685613479133, 45.02656532858658522 ) ) ;
#11356 = DIRECTION ( 'NONE',  ( -3.063596499322173499E-16, 0.000000000000000000, 1.000000000000000000 ) ) ;
#11357 = EDGE_CURVE ( 'NONE', #19508, #17407, #20957, .T. ) ;
#11358 = ORIENTED_EDGE ( 'NONE', *, *, #13226, .F. ) ;
#11359 = ORIENTED_EDGE ( 'NONE', *, *, #11690, .F. ) ;
#11360 = ORIENTED_EDGE ( 'NONE', *, *, #1728, .T. ) ;
#11361 = CARTESIAN_POINT ( 'NONE',  ( 11.51554440985536054, 39.99999999999998579, 54.14601575511818510 ) ) ;
#11362 = CARTESIAN_POINT ( 'NONE',  ( 7.682546357462705089, -2.941798577944364723, 52.37062424969784757 ) ) ;
#11363 = AXIS2_PLACEMENT_3D ( 'NONE', #7704, #18463, #13176 ) ;
#11364 = DIRECTION ( 'NONE',  ( 0.000000000000000000, 0.000000000000000000, -1.000000000000000000 ) ) ;
#11365 = CARTESIAN_POINT ( 'NONE',  ( -42.50000000000000711, -12.00000000000000000, -41.00000000000000000 ) ) ;
#11366 = CARTESIAN_POINT ( 'NONE',  ( -2.814138792736986665E-14, -0.3324270965933693867, 47.91030067221368682 ) ) ;
#11367 = VERTEX_POINT ( 'NONE', #9154 ) ;
#11368 = DIRECTION ( 'NONE',  ( 1.000000000000000000, -1.301042606982605814E-16, 0.000000000000000000 ) ) ;
#11369 = CYLINDRICAL_SURFACE ( 'NONE', #6140, 19.11328065563151668 ) ;
#11370 = ORIENTED_EDGE ( 'NONE', *, *, #21564, .F. ) ;
#11371 = DIRECTION ( 'NONE',  ( -6.505213034913038160E-19, -3.903127820947822896E-18, -1.000000000000000000 ) ) ;
#11372 = CARTESIAN_POINT ( 'NONE',  ( 2.220446049250313081E-13, -8.326672684688674053E-14, 2.800654218530498785 ) ) ;
#11373 = CARTESIAN_POINT ( 'NONE',  ( 3.179547380502777187, 39.99999999999999289, 50.65098720036137081 ) ) ;
#11374 = ORIENTED_EDGE ( 'NONE', *, *, #18233, .F. ) ;
#11375 = FACE_OUTER_BOUND ( 'NONE', #13366, .T. ) ;
#11376 = CARTESIAN_POINT ( 'NONE',  ( -0.3446551741050853934, -0.009348518860262763908, 50.24945914274604064 ) ) ;
#11377 = VERTEX_POINT ( 'NONE', #1935 ) ;
#11378 = LINE ( 'NONE', #12971, #2057 ) ;
#11379 = EDGE_CURVE ( 'NONE', #19741, #4643, #6362, .T. ) ;
#11380 = VERTEX_POINT ( 'NONE', #12685 ) ;
#11381 = CARTESIAN_POINT ( 'NONE',  ( 14.77818138858686048, 33.48299671874048045, 59.09975138256965010 ) ) ;
#11382 = FACE_OUTER_BOUND ( 'NONE', #10498, .T. ) ;
#11383 = DIRECTION ( 'NONE',  ( 6.505213034913038160E-19, 3.903127820947822896E-18, 1.000000000000000000 ) ) ;
#11384 = EDGE_CURVE ( 'NONE', #22334, #17065, #5269, .T. ) ;
#11385 = VECTOR ( 'NONE', #12647, 1000.000000000000000 ) ;
#11386 = CARTESIAN_POINT ( 'NONE',  ( 17.17026400045398304, 34.49621688465821023, -57.29349885535136622 ) ) ;
#11387 = B_SPLINE_CURVE_WITH_KNOTS ( 'NONE', 3,
 ( #12469, #19482, #3786, #19380, #17755, #9052, #16031, #341, #6188, #16375, #2408, #4364, #14648, #11215, #2750, #21655, #11866, #7905, #911, #5845, #20281, #9731, #11340, #5952, #1454, #13152, #692, #12922, #18325, #19934, #18215, #16719, #4242, #10141, #14866, #17136, #8438, #4892, #7783, #1024, #2528, #9513, #21548, #20165, #13034, #12813, #11448, #11101, #6294, #19826, #13253, #16492, #18435, #800, #14757, #4127, #21772 ),
 .UNSPECIFIED., .F., .F.,
 ( 4, 2, 1, 1, 1, 2, 2, 2, 1, 1, 1, 2, 2, 2, 1, 1, 1, 2, 2, 2, 1, 1, 1, 1, 2, 2, 2, 1, 1, 1, 1, 1, 1, 2, 2, 2, 2, 4 ),
 ( 0.0001220703125000000000, 0.01574516296389847497, 0.02355670928959713653, 0.02746248245244646904, 0.02941536903387057672, 0.03039181232458206330, 0.03136825561529354989, 0.04699134826667931281, 0.05480289459237219080, 0.05870866775521863673, 0.06066155433664183888, 0.06163799762735343302, 0.06261444091806502021, 0.09386062622083597706, 0.1094837188722208726, 0.1172952651979133482, 0.1212010383607589475, 0.1231539249421811366, 0.1251068115236033118, 0.1875991821290926842, 0.2188453674318368292, 0.2344684600832089294, 0.2422800064088944383, 0.2461857795717378450, 0.2481386661531595761, 0.2500915527345812794, 0.3750762939455960510, 0.4375686645511029371, 0.4688148498538569631, 0.4844379425052339205, 0.4922494888309228989, 0.4961552619937668052, 0.4981081485751883142, 0.4990845918658983749, 0.5000610351566083800, 0.6250457763674563960, 0.7500305175783041900, 1.000000000000000000 ),
 .UNSPECIFIED. ) ;
#11388 = ORIENTED_EDGE ( 'NONE', *, *, #4356, .T. ) ;
#11389 = EDGE_LOOP ( 'NONE', ( #5473, #8116, #5349, #11618, #16548 ) ) ;
#11390 = VERTEX_POINT ( 'NONE', #14637 ) ;
#11391 = ORIENTED_EDGE ( 'NONE', *, *, #7511, .F. ) ;
#11392 = CARTESIAN_POINT ( 'NONE',  ( 15.49999999999993960, 42.51666049839543149, -105.0000000000000142 ) ) ;
#11393 = AXIS2_PLACEMENT_3D ( 'NONE', #13955, #8263, #15350 ) ;
#11394 = AXIS2_PLACEMENT_3D ( 'NONE', #6773, #13737, #10415 ) ;
#11395 = DIRECTION ( 'NONE',  ( 6.505213034913038160E-19, 3.903127820947822896E-18, 1.000000000000000000 ) ) ;
#11396 = EDGE_CURVE ( 'NONE', #10145, #19815, #18541, .T. ) ;
#11397 = VERTEX_POINT ( 'NONE', #4349 ) ;
#11398 = DIRECTION ( 'NONE',  ( 1.000000000000000000, 0.000000000000000000, 0.000000000000000000 ) ) ;
#11399 = DIRECTION ( 'NONE',  ( 0.000000000000000000, 0.000000000000000000, 1.000000000000000000 ) ) ;
#11400 = ORIENTED_EDGE ( 'NONE', *, *, #1264, .T. ) ;
#11401 = CARTESIAN_POINT ( 'NONE',  ( -1.572625745562107324, 13.32985487263445812, 8.879522542764194171 ) ) ;
#11402 = ORIENTED_EDGE ( 'NONE', *, *, #15894, .T. ) ;
#11403 = FACE_OUTER_BOUND ( 'NONE', #7607, .T. ) ;
#11404 = EDGE_CURVE ( 'NONE', #16804, #5777, #8197, .T. ) ;
#11405 = CARTESIAN_POINT ( 'NONE',  ( -35.00000000000000711, 14.00000000000000000, -38.99999999999997868 ) ) ;
#11406 = EDGE_CURVE ( 'NONE', #14574, #8378, #7890, .T. ) ;
#11407 = CARTESIAN_POINT ( 'NONE',  ( -34.99999999999998579, 0.000000000000000000, 58.99999999999695888 ) ) ;
#11408 = CIRCLE ( 'NONE', #15416, 58.99999999999699440 ) ;
#11409 = CARTESIAN_POINT ( 'NONE',  ( -1.575030625093513326, 39.98856684152734431, 49.93404140185739948 ) ) ;
#11410 = LINE ( 'NONE', #14948, #6093 ) ;
#11411 = EDGE_CURVE ( 'NONE', #19815, #2292, #11852, .T. ) ;
#11412 = ORIENTED_EDGE ( 'NONE', *, *, #8991, .T. ) ;
#11413 = ORIENTED_EDGE ( 'NONE', *, *, #6617, .T. ) ;
#11414 = EDGE_CURVE ( 'NONE', #11797, #3437, #9601, .T. ) ;
#11415 = EDGE_LOOP ( 'NONE', ( #15156, #813, #20482, #9341 ) ) ;
#11416 = CARTESIAN_POINT ( 'NONE',  ( -20.01613897799924047, 20.29830884309395600, 58.15166638929883192 ) ) ;
#11417 = CARTESIAN_POINT ( 'NONE',  ( 2.220446049250313081E-13, -8.326672684688674053E-14, 2.800654218530498785 ) ) ;
#11418 = EDGE_CURVE ( 'NONE', #5124, #18180, #1440, .T. ) ;
#11419 = FACE_OUTER_BOUND ( 'NONE', #14791, .T. ) ;
#11420 = CARTESIAN_POINT ( 'NONE',  ( -6.070730550690850436, -31.88709182564697286, 3.000000000000023537 ) ) ;
#11421 = B_SPLINE_CURVE_WITH_KNOTS ( 'NONE', 3,
 ( #11171, #2595, #21725, #9805, #6144, #21967 ),
 .UNSPECIFIED., .F., .F.,
 ( 4, 2, 4 ),
 ( 0.000000000000000000, 0.2500000000000000000, 0.5000000000000000000 ),
 .UNSPECIFIED. ) ;
#11422 = AXIS2_PLACEMENT_3D ( 'NONE', #13042, #2985, #21780 ) ;
#11423 = DIRECTION ( 'NONE',  ( 0.000000000000000000, 1.000000000000000000, 0.000000000000000000 ) ) ;
#11424 = CARTESIAN_POINT ( 'NONE',  ( 35.00000000000001421, 5.000000000000000000, 9.000000000000035527 ) ) ;
#11425 = CARTESIAN_POINT ( 'NONE',  ( -35.00000000000000000, 14.00000000000000000, 39.00000000000002132 ) ) ;
#11426 = DIRECTION ( 'NONE',  ( -0.000000000000000000, -1.000000000000000000, -0.000000000000000000 ) ) ;
#11427 = CARTESIAN_POINT ( 'NONE',  ( -3.244689583143077094, 39.74755540027242517, -52.34195286441636341 ) ) ;
#11428 = ADVANCED_FACE ( 'NONE', ( #8426 ), #11203, .F. ) ;
#11429 = CARTESIAN_POINT ( 'NONE',  ( 24.24871130596442725, 14.00000000000009592, -2.999999999999947153 ) ) ;
#11430 = VERTEX_POINT ( 'NONE', #9388 ) ;
#11431 = LINE ( 'NONE', #9497, #6359 ) ;
#11432 = DIRECTION ( 'NONE',  ( 0.000000000000000000, 0.000000000000000000, 1.000000000000000000 ) ) ;
#11433 = CARTESIAN_POINT ( 'NONE',  ( 1.734723475976807094E-14, 20.00000000000000000, 20.71067811865476216 ) ) ;
#11434 = DIRECTION ( 'NONE',  ( 0.000000000000000000, 0.000000000000000000, 1.000000000000000000 ) ) ;
#11435 = ADVANCED_FACE ( 'NONE', ( #20154 ), #16361, .F. ) ;
#11436 = ORIENTED_EDGE ( 'NONE', *, *, #646, .T. ) ;
#11437 = ORIENTED_EDGE ( 'NONE', *, *, #3180, .T. ) ;
#11438 = DIRECTION ( 'NONE',  ( 0.000000000000000000, 1.000000000000000000, 0.000000000000000000 ) ) ;
#11439 = CARTESIAN_POINT ( 'NONE',  ( 42.50000000000000711, -12.00000000000000000, -47.50000000000000000 ) ) ;
#11440 = EDGE_CURVE ( 'NONE', #15106, #12187, #17703, .T. ) ;
#11441 = CIRCLE ( 'NONE', #14352, 2.000000000000000888 ) ;
#11442 = AXIS2_PLACEMENT_3D ( 'NONE', #7508, #17932, #3848 ) ;
#11443 = ORIENTED_EDGE ( 'NONE', *, *, #21508, .T. ) ;
#11444 = AXIS2_PLACEMENT_3D ( 'NONE', #13305, #20329, #1294 ) ;
#11445 = CARTESIAN_POINT ( 'NONE',  ( -42.50000000000000711, -9.600000000000001421, 50.00000000000000711 ) ) ;
#11446 = FACE_OUTER_BOUND ( 'NONE', #9833, .T. ) ;
#11447 = ORIENTED_EDGE ( 'NONE', *, *, #6730, .T. ) ;
#11448 = CARTESIAN_POINT ( 'NONE',  ( 4.577493544539172454, 39.86955222714477998, -51.95007588729110637 ) ) ;
#11449 = CARTESIAN_POINT ( 'NONE',  ( -29.33526866242075570, 22.15900668633760517, -1.999999999999977573 ) ) ;
#11450 = CARTESIAN_POINT ( 'NONE',  ( -9.999999999999998224, 12.49999999999999822, -3.000000000000000000 ) ) ;
#11451 = LINE ( 'NONE', #16610, #5413 ) ;
#11452 = CARTESIAN_POINT ( 'NONE',  ( 9.689843208404422370, 39.33333333333334281, -54.54983754392748097 ) ) ;
#11453 = CARTESIAN_POINT ( 'NONE',  ( -8.845639221078089420, 39.99999999999999289, 53.28397946285252829 ) ) ;
#11454 = CIRCLE ( 'NONE', #10348, 19.11328065563151668 ) ;
#11455 = CARTESIAN_POINT ( 'NONE',  ( -34.99999999999999289, 1.000000000000044187, -10.00000000000003020 ) ) ;
#11456 = ORIENTED_EDGE ( 'NONE', *, *, #13735, .T. ) ;
#11457 = CARTESIAN_POINT ( 'NONE',  ( 2.602085213965210642E-15, 6.000000000000019540, 0.000000000000000000 ) ) ;
#11458 = CYLINDRICAL_SURFACE ( 'NONE', #22118, 31.50000000000001421 ) ;
#11459 = CARTESIAN_POINT ( 'NONE',  ( 34.99999999999999289, -5.000000000000000000, -54.99999999999705835 ) ) ;
#11460 = VECTOR ( 'NONE', #12515, 1000.000000000000000 ) ;
#11461 = DIRECTION ( 'NONE',  ( -1.445602896647339410E-16, -0.000000000000000000, -1.000000000000000000 ) ) ;
#11462 = CARTESIAN_POINT ( 'NONE',  ( 29.99999999999998579, 20.00000000000000355, -100.0000000000000000 ) ) ;
#11463 = VECTOR ( 'NONE', #6916, 1000.000000000000114 ) ;
#11464 = ADVANCED_FACE ( 'NONE', ( #6175 ), #4458, .T. ) ;
#11465 = EDGE_LOOP ( 'NONE', ( #16757, #17531, #15690, #1629, #6862, #4873 ) ) ;
#11466 = CARTESIAN_POINT ( 'NONE',  ( -25.00000000000000000, -20.00000000000000000, -16.49999999999998934 ) ) ;
#11467 = CARTESIAN_POINT ( 'NONE',  ( -26.00000000000001421, 19.99999999999982947, -105.0000000000000142 ) ) ;
#11468 = EDGE_CURVE ( 'NONE', #5292, #16920, #4180, .T. ) ;
#11469 = ORIENTED_EDGE ( 'NONE', *, *, #8327, .T. ) ;
#11470 = CIRCLE ( 'NONE', #4539, 2.500000000000002220 ) ;
#11471 = ORIENTED_EDGE ( 'NONE', *, *, #2899, .F. ) ;
#11472 = AXIS2_PLACEMENT_3D ( 'NONE', #8816, #5591, #2049 ) ;
#11473 = CARTESIAN_POINT ( 'NONE',  ( 0.000000000000000000, 0.000000000000000000, 0.000000000000000000 ) ) ;
#11474 = AXIS2_PLACEMENT_3D ( 'NONE', #18084, #7433, #19475 ) ;
#11475 = VERTEX_POINT ( 'NONE', #5938 ) ;
#11476 = CARTESIAN_POINT ( 'NONE',  ( 19.91015268464080279, 21.95549706463424400, 60.60051340835966016 ) ) ;
#11477 = DIRECTION ( 'NONE',  ( -0.000000000000000000, -1.000000000000000000, -0.000000000000000000 ) ) ;
#11478 = CARTESIAN_POINT ( 'NONE',  ( -2.999999999999998668, 22.79887287893604153, 8.485281374238567764 ) ) ;
#11479 = DIRECTION ( 'NONE',  ( 1.296372316667914327E-16, 1.000000000000000000, -0.000000000000000000 ) ) ;
#11480 = CARTESIAN_POINT ( 'NONE',  ( -4.108808078302945255, 5.537732191391603997, -39.55687577697710822 ) ) ;
#11481 = VERTEX_POINT ( 'NONE', #788 ) ;
#11482 = CARTESIAN_POINT ( 'NONE',  ( -15.02862401740787135, -32.75570538720795355, -2.999999999999971578 ) ) ;
#11483 = LINE ( 'NONE', #16756, #635 ) ;
#11484 = ORIENTED_EDGE ( 'NONE', *, *, #8839, .T. ) ;
#11485 = CARTESIAN_POINT ( 'NONE',  ( -42.50000000000000711, -12.00000000000000000, 54.00000000000000711 ) ) ;
#11486 = CARTESIAN_POINT ( 'NONE',  ( -22.16820537380702660, 16.50892643625844158, -58.61209530626887698 ) ) ;
#11487 = EDGE_CURVE ( 'NONE', #2202, #20150, #19902, .T. ) ;
#11488 = CARTESIAN_POINT ( 'NONE',  ( 7.298342794717536198E-15, -4.765964690023824168, 45.28512947536575695 ) ) ;
#11489 = VECTOR ( 'NONE', #4095, 1000.000000000000000 ) ;
#11490 = CARTESIAN_POINT ( 'NONE',  ( 12.89955995983991421, 4.696256998628590473, -58.40693116658149364 ) ) ;
#11491 = ORIENTED_EDGE ( 'NONE', *, *, #14660, .T. ) ;
#11492 = DIRECTION ( 'NONE',  ( -0.000000000000000000, 1.000000000000000000, -0.000000000000000000 ) ) ;
#11493 = CARTESIAN_POINT ( 'NONE',  ( -35.00000000000000000, 17.00000000000000000, -16.99999999999997868 ) ) ;
#11494 = ORIENTED_EDGE ( 'NONE', *, *, #11640, .T. ) ;
#11495 = DIRECTION ( 'NONE',  ( 0.000000000000000000, 0.000000000000000000, 1.000000000000000000 ) ) ;
#11496 = FACE_OUTER_BOUND ( 'NONE', #18730, .T. ) ;
#11497 = CARTESIAN_POINT ( 'NONE',  ( -3.095776913249378250E-14, -0.8525976281474469953, -48.47768327036356339 ) ) ;
#11498 = EDGE_LOOP ( 'NONE', ( #3052, #2815, #360, #21297 ) ) ;
#11499 = UNCERTAINTY_MEASURE_WITH_UNIT (LENGTH_MEASURE( 1.000000000000000082E-05 ), #15604, 'distance_accuracy_value', 'NONE');
#11500 = AXIS2_PLACEMENT_3D ( 'NONE', #13029, #18321, #14862 ) ;
#11501 = CARTESIAN_POINT ( 'NONE',  ( 35.79662727779903264, -4.171001175319571708, 2.999999999999999112 ) ) ;
#11502 = FACE_OUTER_BOUND ( 'NONE', #13395, .T. ) ;
#11503 = CONICAL_SURFACE ( 'NONE', #7836, 2.524999999999999467, 0.7853981633974482790 ) ;
#11504 = CARTESIAN_POINT ( 'NONE',  ( 21.32594275109616433, 27.02633437841368291, -58.42208514511779072 ) ) ;
#11505 = ORIENTED_EDGE ( 'NONE', *, *, #2745, .T. ) ;
#11506 = APPLICATION_CONTEXT ( 'automotive_design' ) ;
#11507 = ORIENTED_EDGE ( 'NONE', *, *, #5139, .F. ) ;
#11508 = VECTOR ( 'NONE', #17992, 1000.000000000000000 ) ;
#11509 = ORIENTED_EDGE ( 'NONE', *, *, #18187, .T. ) ;
#11510 = ADVANCED_FACE ( 'NONE', ( #4116 ), #12908, .T. ) ;
#11511 = ORIENTED_EDGE ( 'NONE', *, *, #15443, .T. ) ;
#11512 = FACE_OUTER_BOUND ( 'NONE', #20109, .T. ) ;
#11513 = CARTESIAN_POINT ( 'NONE',  ( 4.918774254215884767, -31.11359284679388182, -7.000000000000006217 ) ) ;
#11514 = PRODUCT_DEFINITION_SHAPE ( 'NONE', 'NONE',  #17241 ) ;
#11515 = ORIENTED_EDGE ( 'NONE', *, *, #5798, .F. ) ;
#11516 = CARTESIAN_POINT ( 'NONE',  ( -27.56232195404058416, 21.41958700883256483, 2.999999999999995559 ) ) ;
#11517 = CARTESIAN_POINT ( 'NONE',  ( 2.396330562594276348, 14.15354796518962388, 6.679745199225937569 ) ) ;
#11518 = ORIENTED_EDGE ( 'NONE', *, *, #18288, .F. ) ;
#11519 = CARTESIAN_POINT ( 'NONE',  ( 0.7857880201000516651, 12.99916404495074040, 9.000278651543345276 ) ) ;
#11520 = PRESENTATION_LAYER_ASSIGNMENT (  '', '', ( #7851 ) ) ;
#11521 = EDGE_CURVE ( 'NONE', #19192, #17751, #14967, .T. ) ;
#11522 = ORIENTED_EDGE ( 'NONE', *, *, #11211, .T. ) ;
#11523 = CARTESIAN_POINT ( 'NONE',  ( 35.00000000000001421, -1.000000000000028644, 59.99999999999703704 ) ) ;
#11524 = CARTESIAN_POINT ( 'NONE',  ( 9.184850993605147944E-16, 30.00000000000000000, 7.500000000000000000 ) ) ;
#11525 = LINE ( 'NONE', #13113, #5343 ) ;
#11526 = CARTESIAN_POINT ( 'NONE',  ( -12.99999999999999467, -20.00000000000000000, 11.32475165290612296 ) ) ;
#11527 = CARTESIAN_POINT ( 'NONE',  ( -14.98515767422211198, 19.22844023086510745, 45.81928800960655934 ) ) ;
#11528 = EDGE_CURVE ( 'NONE', #4626, #19154, #20628, .T. ) ;
#11529 = ORIENTED_EDGE ( 'NONE', *, *, #2612, .T. ) ;
#11530 = VERTEX_POINT ( 'NONE', #20267 ) ;
#11531 = AXIS2_PLACEMENT_3D ( 'NONE', #9449, #11269, #4409 ) ;
#11532 = EDGE_CURVE ( 'NONE', #4643, #19741, #13664, .T. ) ;
#11533 = EDGE_LOOP ( 'NONE', ( #5214, #14667, #7244, #17815 ) ) ;
#11534 = CARTESIAN_POINT ( 'NONE',  ( -19.43475998741692834, 8.756352882855134467, 57.94642939675672721 ) ) ;
#11535 = DIRECTION ( 'NONE',  ( -6.505213034913038160E-19, -3.903127820947822896E-18, -1.000000000000000000 ) ) ;
#11536 = DIRECTION ( 'NONE',  ( 0.000000000000000000, 0.000000000000000000, -1.000000000000000000 ) ) ;
#11537 = CARTESIAN_POINT ( 'NONE',  ( -11.19713514086471129, 39.99999999999999289, 54.03748032825711078 ) ) ;
#11538 = CIRCLE ( 'NONE', #7522, 1.999999999999999778 ) ;
#11539 = PLANE ( 'NONE',  #10455 ) ;
#11540 = DIRECTION ( 'NONE',  ( 0.000000000000000000, 0.000000000000000000, -1.000000000000000000 ) ) ;
#11541 = FACE_OUTER_BOUND ( 'NONE', #3510, .T. ) ;
#11542 = CARTESIAN_POINT ( 'NONE',  ( 32.89708536800427652, 15.00428685838163823, 2.932460736555811742 ) ) ;
#11543 = CARTESIAN_POINT ( 'NONE',  ( 3.235223465813951371, -4.647308930658565096, 47.76313845446021134 ) ) ;
#11544 = DIRECTION ( 'NONE',  ( -0.000000000000000000, 1.000000000000000000, -0.000000000000000000 ) ) ;
#11545 = EDGE_LOOP ( 'NONE', ( #16672, #13613, #7819, #20523 ) ) ;
#11546 = LINE ( 'NONE', #22097, #7316 ) ;
#11547 = CARTESIAN_POINT ( 'NONE',  ( 16.37028666999325210, 4.520534895872216907, 57.04777702420265939 ) ) ;
#11548 = CIRCLE ( 'NONE', #6427, 30.00000000000000000 ) ;
#11549 = DIRECTION ( 'NONE',  ( -0.000000000000000000, -0.000000000000000000, 1.000000000000000000 ) ) ;
#11550 = VERTEX_POINT ( 'NONE', #10350 ) ;
#11551 = CIRCLE ( 'NONE', #6795, 19.11328065563150957 ) ;
#11552 = CARTESIAN_POINT ( 'NONE',  ( -35.00000000000058265, 40.00000000000000000, -57.50000000000076028 ) ) ;
#11553 = EDGE_CURVE ( 'NONE', #8231, #19408, #12418, .T. ) ;
#11554 = DIRECTION ( 'NONE',  ( 0.000000000000000000, 0.000000000000000000, 1.000000000000000000 ) ) ;
#11555 = FACE_OUTER_BOUND ( 'NONE', #212, .T. ) ;
#11556 = VECTOR ( 'NONE', #15364, 1000.000000000000000 ) ;
#11557 = AXIS2_PLACEMENT_3D ( 'NONE', #11194, #19912, #21870 ) ;
#11558 = ADVANCED_FACE ( 'NONE', ( #7043 ), #9980, .T. ) ;
#11559 = ADVANCED_FACE ( 'NONE', ( #1549 ), #2001, .F. ) ;
#11560 = ADVANCED_FACE ( 'NONE', ( #13904, #3284 ), #156, .T. ) ;
#11561 = DIRECTION ( 'NONE',  ( 1.000000000000000000, 2.269002777743560714E-17, 0.000000000000000000 ) ) ;
#11562 = CARTESIAN_POINT ( 'NONE',  ( 0.7906703573358260240, 40.00000000000000000, -49.24721022140938231 ) ) ;
#11563 = AXIS2_PLACEMENT_3D ( 'NONE', #7876, #6496, #21866 ) ;
#11564 = AXIS2_PLACEMENT_3D ( 'NONE', #10345, #18968, #3278 ) ;
#11565 = VERTEX_POINT ( 'NONE', #12311 ) ;
#11566 = VECTOR ( 'NONE', #11461, 1000.000000000000000 ) ;
#11567 = CARTESIAN_POINT ( 'NONE',  ( 35.00000000000001421, -1.000000000000028644, 1.540743955509788682E-30 ) ) ;
#11568 = ADVANCED_FACE ( 'NONE', ( #6706, #3625 ), #19201, .F. ) ;
#11569 = LINE ( 'NONE', #18555, #1921 ) ;
#11570 = DIRECTION ( 'NONE',  ( 0.000000000000000000, 0.000000000000000000, 1.000000000000000000 ) ) ;
#11571 = DIRECTION ( 'NONE',  ( 1.000000000000000000, 1.208970125616063182E-17, 0.000000000000000000 ) ) ;
#11572 = LINE ( 'NONE', #13258, #11168 ) ;
#11573 = VECTOR ( 'NONE', #22685, 1000.000000000000000 ) ;
#11574 = CARTESIAN_POINT ( 'NONE',  ( 42.50000000000000711, -9.600000000000001421, -45.40000000000000568 ) ) ;
#11575 = ORIENTED_EDGE ( 'NONE', *, *, #3874, .T. ) ;
#11576 = CARTESIAN_POINT ( 'NONE',  ( -14.76298474240489433, -28.95348479018575105, -2.999999999999971578 ) ) ;
#11577 = CARTESIAN_POINT ( 'NONE',  ( -19.99999999999982236, -5.551115123125782702E-14, 3.000000000000016431 ) ) ;
#11578 = CARTESIAN_POINT ( 'NONE',  ( 10.31465995609163322, 2.846668092512274484, -57.27881138850304410 ) ) ;
#11579 = CARTESIAN_POINT ( 'NONE',  ( -35.00000000000000000, 0.000000000000000000, 41.00000000000002132 ) ) ;
#11580 = VERTEX_POINT ( 'NONE', #11974 ) ;
#11581 = DIRECTION ( 'NONE',  ( 1.000000000000000000, -1.275531967630005245E-16, 0.000000000000000000 ) ) ;
#11582 = DIRECTION ( 'NONE',  ( -0.000000000000000000, -1.000000000000000000, 0.000000000000000000 ) ) ;
#11583 = DIRECTION ( 'NONE',  ( -1.000000000000000000, -1.208970125616046080E-17, 6.505213034913038160E-19 ) ) ;
#11584 = AXIS2_PLACEMENT_3D ( 'NONE', #14912, #18022, #2683 ) ;
#11585 = ORIENTED_EDGE ( 'NONE', *, *, #9396, .F. ) ;
#11586 = AXIS2_PLACEMENT_3D ( 'NONE', #11180, #9693, #13119 ) ;
#11587 = ORIENTED_EDGE ( 'NONE', *, *, #9014, .F. ) ;
#11588 = CARTESIAN_POINT ( 'NONE',  ( 153.3614336593539349, 176.6809246203112309, -16.64187286134538724 ) ) ;
#11589 = EDGE_CURVE ( 'NONE', #16318, #4151, #19316, .T. ) ;
#11590 = ORIENTED_EDGE ( 'NONE', *, *, #17744, .F. ) ;
#11591 = CARTESIAN_POINT ( 'NONE',  ( 8.331955809010596070, 38.18181818181818699, -56.36098470834070895 ) ) ;
#11592 = DIRECTION ( 'NONE',  ( 0.000000000000000000, -1.000000000000000000, 0.000000000000000000 ) ) ;
#11593 = CARTESIAN_POINT ( 'NONE',  ( 21.65063509461090518, 12.49999999999978861, 2.999999999999995559 ) ) ;
#11594 = ADVANCED_FACE ( 'NONE', ( #8651 ), #20807, .F. ) ;
#11595 = CARTESIAN_POINT ( 'NONE',  ( 15.59166974688843688, 7.467814210042471146, 59.37578565761233307 ) ) ;
#11596 = ORIENTED_EDGE ( 'NONE', *, *, #182, .T. ) ;
#11597 = CARTESIAN_POINT ( 'NONE',  ( -15.12081897056651059, 33.51030287062345536, 2.800654218530485018 ) ) ;
#11598 = CARTESIAN_POINT ( 'NONE',  ( -35.00000000000000000, 2.142135623730931471, 1.387778780781445676E-14 ) ) ;
#11599 = VERTEX_POINT ( 'NONE', #15626 ) ;
#11600 = LINE ( 'NONE', #18595, #22603 ) ;
#11601 = CARTESIAN_POINT ( 'NONE',  ( -6.696867368503558448E-15, 39.00000000000000711, -48.73397172404479960 ) ) ;
#11602 = CARTESIAN_POINT ( 'NONE',  ( 6.447719747032748441E-15, -4.883049072963745019, 45.13706194851797449 ) ) ;
#11603 = CARTESIAN_POINT ( 'NONE',  ( -34.88850421923971368, 1.128083539116031542, -2.999999999999981792 ) ) ;
#11604 = ORIENTED_EDGE ( 'NONE', *, *, #12937, .T. ) ;
#11605 = CARTESIAN_POINT ( 'NONE',  ( -5.249999999999978684, 40.00000000000000000, 41.42387596543811412 ) ) ;
#11606 = FACE_OUTER_BOUND ( 'NONE', #11303, .T. ) ;
#11607 = EDGE_CURVE ( 'NONE', #22470, #3870, #15450, .T. ) ;
#11608 = EDGE_LOOP ( 'NONE', ( #15168, #9261, #4828, #15573 ) ) ;
#11609 = DIRECTION ( 'NONE',  ( -6.505213034913038160E-19, -3.903127820947822896E-18, -1.000000000000000000 ) ) ;
#11610 = CARTESIAN_POINT ( 'NONE',  ( -6.976621346229579856, 1.175841510106858667, -53.23008234738043853 ) ) ;
#11611 = ORIENTED_EDGE ( 'NONE', *, *, #22321, .T. ) ;
#11612 = LINE ( 'NONE', #13876, #18116 ) ;
#11613 = CARTESIAN_POINT ( 'NONE',  ( -28.52469787935782364, 10.00000000000000000, 4.095854054471899985 ) ) ;
#11614 = AXIS2_PLACEMENT_3D ( 'NONE', #8636, #10339, #15615 ) ;
#11615 = CARTESIAN_POINT ( 'NONE',  ( 17.19628968518533085, 9.778502620742363760, -59.87797704339183724 ) ) ;
#11616 = AXIS2_PLACEMENT_3D ( 'NONE', #13183, #4742, #12964 ) ;
#11617 = ORIENTED_EDGE ( 'NONE', *, *, #19164, .F. ) ;
#11618 = ORIENTED_EDGE ( 'NONE', *, *, #7957, .T. ) ;
#11619 = ORIENTED_EDGE ( 'NONE', *, *, #7958, .T. ) ;
#11620 = ORIENTED_EDGE ( 'NONE', *, *, #10332, .F. ) ;
#11621 = CARTESIAN_POINT ( 'NONE',  ( -89.99999999999701572, -5.000000000000000000, -2.500000000000038636 ) ) ;
#11622 = ORIENTED_EDGE ( 'NONE', *, *, #5084, .F. ) ;
#11623 = DIRECTION ( 'NONE',  ( 0.000000000000000000, 0.000000000000000000, -1.000000000000000000 ) ) ;
#11624 = CARTESIAN_POINT ( 'NONE',  ( -8.460114887485421065, -4.900635314995738234, -50.56657553899492541 ) ) ;
#11625 = ORIENTED_EDGE ( 'NONE', *, *, #19194, .T. ) ;
#11626 = CARTESIAN_POINT ( 'NONE',  ( 32.40961249803578426, -2.422192751864060689, -6.999999999999950262 ) ) ;
#11627 = CIRCLE ( 'NONE', #21510, 1.000000000000000888 ) ;
#11628 = DIRECTION ( 'NONE',  ( -1.000000000000000000, 1.084202172485505420E-16, 0.000000000000000000 ) ) ;
#11629 = ORIENTED_EDGE ( 'NONE', *, *, #4537, .T. ) ;
#11630 = CARTESIAN_POINT ( 'NONE',  ( 5.340789179572837497, 39.27722415257166233, -54.28402915905239468 ) ) ;
#11631 = DIRECTION ( 'NONE',  ( -0.000000000000000000, -1.000000000000000000, -0.000000000000000000 ) ) ;
#11632 = CARTESIAN_POINT ( 'NONE',  ( -6.777919286276303216E-15, -4.184616259352855749, -46.01897913074525803 ) ) ;
#11633 = CIRCLE ( 'NONE', #2494, 1.000000000000000888 ) ;
#11634 = DIRECTION ( 'NONE',  ( -1.000000000000000000, -1.208970125616060101E-17, 6.505213034913038160E-19 ) ) ;
#11635 = EDGE_CURVE ( 'NONE', #20449, #4414, #19083, .T. ) ;
#11636 = CARTESIAN_POINT ( 'NONE',  ( 10.99584631063768647, 3.272668205460784741, -57.61971594758620796 ) ) ;
#11637 = CIRCLE ( 'NONE', #7253, 0.9999999999999991118 ) ;
#11638 = ORIENTED_EDGE ( 'NONE', *, *, #3834, .F. ) ;
#11639 = VECTOR ( 'NONE', #17112, 1000.000000000000000 ) ;
#11640 = EDGE_CURVE ( 'NONE', #12190, #17561, #15509, .T. ) ;
#11641 = CIRCLE ( 'NONE', #10527, 3.999999999999998224 ) ;
#11642 = ORIENTED_EDGE ( 'NONE', *, *, #13505, .F. ) ;
#11643 = AXIS2_PLACEMENT_3D ( 'NONE', #18284, #2821, #2362 ) ;
#11644 = TOROIDAL_SURFACE ( 'NONE', #17862, 34.90673715956759082, 8.750000000000000000 ) ;
#11645 = ORIENTED_EDGE ( 'NONE', *, *, #6094, .F. ) ;
#11646 = CARTESIAN_POINT ( 'NONE',  ( -14.30107462755440473, 5.991811841696772944, 58.93430465799253426 ) ) ;
#11647 = DIRECTION ( 'NONE',  ( 6.505213034913038160E-19, 3.903127820947822896E-18, 1.000000000000000000 ) ) ;
#11648 = CARTESIAN_POINT ( 'NONE',  ( 0.000000000000000000, 30.00000000000000355, 0.000000000000000000 ) ) ;
#11649 = CARTESIAN_POINT ( 'NONE',  ( 42.49999999999998579, 10.00000000000000000, -44.99999999999997868 ) ) ;
#11650 = EDGE_CURVE ( 'NONE', #586, #7599, #1569, .T. ) ;
#11651 = CIRCLE ( 'NONE', #4357, 0.9999999999999974465 ) ;
#11652 = VERTEX_POINT ( 'NONE', #13791 ) ;
#11653 = DIRECTION ( 'NONE',  ( 0.1421319796954322034, 0.000000000000000000, 0.9898477157360405787 ) ) ;
#11654 = DIRECTION ( 'NONE',  ( 1.000000000000000000, 0.000000000000000000, 0.000000000000000000 ) ) ;
#11655 = DIRECTION ( 'NONE',  ( -1.000000000000000000, 0.000000000000000000, 0.000000000000000000 ) ) ;
#11656 = CARTESIAN_POINT ( 'NONE',  ( 35.00000000000001421, -5.000000000000000000, 1.540743955509788682E-30 ) ) ;
#11657 = B_SPLINE_CURVE_WITH_KNOTS ( 'NONE', 3,
 ( #10927, #21361, #2228, #7612 ),
 .UNSPECIFIED., .F., .F.,
 ( 4, 4 ),
 ( 9.545285769941151703E-07, 0.001900595205834767999 ),
 .UNSPECIFIED. ) ;
#11658 = AXIS2_PLACEMENT_3D ( 'NONE', #10593, #10365, #17249 ) ;
#11659 = AXIS2_PLACEMENT_3D ( 'NONE', #17850, #544, #7539 ) ;
#11660 = ORIENTED_EDGE ( 'NONE', *, *, #12555, .T. ) ;
#11661 = DIRECTION ( 'NONE',  ( 6.505213034913038160E-19, 3.903127820947822896E-18, 1.000000000000000000 ) ) ;
#11662 = DIRECTION ( 'NONE',  ( 1.000000000000000000, 1.208970125616063028E-17, 0.000000000000000000 ) ) ;
#11663 = EDGE_CURVE ( 'NONE', #4123, #22470, #10688, .T. ) ;
#11664 = AXIS2_PLACEMENT_3D ( 'NONE', #17219, #13883, #5201 ) ;
#11665 = EDGE_LOOP ( 'NONE', ( #3425, #17888, #18014, #8476, #18241, #3697, #7357 ) ) ;
#11666 = FACE_OUTER_BOUND ( 'NONE', #15042, .T. ) ;
#11667 = DIRECTION ( 'NONE',  ( 0.000000000000000000, -1.000000000000000000, 0.000000000000000000 ) ) ;
#11668 = DIRECTION ( 'NONE',  ( 0.000000000000000000, 0.000000000000000000, 1.000000000000000000 ) ) ;
#11669 = DIRECTION ( 'NONE',  ( -0.000000000000000000, 1.000000000000000000, -0.000000000000000000 ) ) ;
#11670 = VERTEX_POINT ( 'NONE', #1788 ) ;
#11671 = EDGE_CURVE ( 'NONE', #20094, #14167, #3765, .T. ) ;
#11672 = AXIS2_PLACEMENT_3D ( 'NONE', #15124, #16755, #13180 ) ;
#11673 = EDGE_LOOP ( 'NONE', ( #8320, #2044, #5923, #11511, #627, #21073, #676, #17999 ) ) ;
#11674 = FACE_OUTER_BOUND ( 'NONE', #17228, .T. ) ;
#11675 = DIRECTION ( 'NONE',  ( 1.000000000000000000, 0.000000000000000000, 0.000000000000000000 ) ) ;
#11676 = ORIENTED_EDGE ( 'NONE', *, *, #3163, .T. ) ;
#11677 = DIRECTION ( 'NONE',  ( -0.000000000000000000, -1.000000000000000000, -0.000000000000000000 ) ) ;
#11678 = EDGE_CURVE ( 'NONE', #21198, #12113, #14002, .T. ) ;
#11679 = DIRECTION ( 'NONE',  ( 6.505213034913038160E-19, 3.903127820947822896E-18, 1.000000000000000000 ) ) ;
#11680 = CYLINDRICAL_SURFACE ( 'NONE', #21892, 2.500000000000002220 ) ;
#11681 = LINE ( 'NONE', #14656, #22626 ) ;
#11682 = DIRECTION ( 'NONE',  ( -1.000000000000000000, 0.000000000000000000, 0.000000000000000000 ) ) ;
#11683 = CARTESIAN_POINT ( 'NONE',  ( 16.99647590252675755, 30.48934413892762052, 3.000000000000019984 ) ) ;
#11684 = MECHANICAL_DESIGN_GEOMETRIC_PRESENTATION_REPRESENTATION (  '', ( #15333 ), #19382 ) ;
#11685 = ORIENTED_EDGE ( 'NONE', *, *, #9046, .F. ) ;
#11686 = DIRECTION ( 'NONE',  ( 6.505213034913038160E-19, 3.903127820947822896E-18, 1.000000000000000000 ) ) ;
#11687 = CARTESIAN_POINT ( 'NONE',  ( 1.942890293094023946E-13, -8.326672684688674053E-14, 5.000000000000000888 ) ) ;
#11688 = DIRECTION ( 'NONE',  ( 0.000000000000000000, -1.000000000000000000, 0.000000000000000000 ) ) ;
#11689 = ADVANCED_FACE ( 'NONE', ( #7150 ), #14121, .T. ) ;
#11690 = EDGE_CURVE ( 'NONE', #16507, #507, #5780, .T. ) ;
#11691 = CARTESIAN_POINT ( 'NONE',  ( -0.06748528862095062864, 39.99997318105867805, -48.78643676837788945 ) ) ;
#11692 = VERTEX_POINT ( 'NONE', #14350 ) ;
#11693 = CARTESIAN_POINT ( 'NONE',  ( 35.00000000000000000, 0.000000000000000000, -38.99999999999997868 ) ) ;
#11694 = CARTESIAN_POINT ( 'NONE',  ( 3.330669073875469621E-13, -1.110223024625156540E-13, -2.999999999999971578 ) ) ;
#11695 = ADVANCED_FACE ( 'NONE', ( #17924 ), #18028, .T. ) ;
#11696 = ORIENTED_EDGE ( 'NONE', *, *, #14205, .F. ) ;
#11697 = CIRCLE ( 'NONE', #9515, 2.099999999999997868 ) ;
#11698 = ORIENTED_EDGE ( 'NONE', *, *, #18376, .T. ) ;
#11699 = ADVANCED_FACE ( 'NONE', ( #14467 ), #14356, .T. ) ;
#11700 = ORIENTED_EDGE ( 'NONE', *, *, #469, .F. ) ;
#11701 = DIRECTION ( 'NONE',  ( -0.000000000000000000, -1.000000000000000000, -0.000000000000000000 ) ) ;
#11702 = DIRECTION ( 'NONE',  ( -0.000000000000000000, -1.000000000000000000, -0.000000000000000000 ) ) ;
#11703 = CARTESIAN_POINT ( 'NONE',  ( -7.463862311150981199, -35.99819890246952525, 2.800654218530485018 ) ) ;
#11704 = CARTESIAN_POINT ( 'NONE',  ( -35.00000000000058265, 40.00000000000000000, -55.00000000000076028 ) ) ;
#11705 = ADVANCED_FACE ( 'NONE', ( #3840 ), #19873, .F. ) ;
#11706 = ORIENTED_EDGE ( 'NONE', *, *, #10020, .F. ) ;
#11707 = CARTESIAN_POINT ( 'NONE',  ( -12.99999999999980282, -2.516660498395516310, -105.0000000000000142 ) ) ;
#11708 = CARTESIAN_POINT ( 'NONE',  ( 18.22261011550294185, 31.92986134326200443, 2.800654218530481465 ) ) ;
#11709 = ORIENTED_EDGE ( 'NONE', *, *, #9920, .F. ) ;
#11710 = LINE ( 'NONE', #2907, #1736 ) ;
#11711 = DIRECTION ( 'NONE',  ( 0.000000000000000000, 0.000000000000000000, 1.000000000000000000 ) ) ;
#11713 = VECTOR ( 'NONE', #18216, 1000.000000000000000 ) ;
#11712 = DIRECTION ( 'NONE',  ( -0.000000000000000000, 1.000000000000000000, 0.000000000000000000 ) ) ;
#11714 = CARTESIAN_POINT ( 'NONE',  ( 5.234365386614148186, 40.00000000000000711, 51.72901478475910153 ) ) ;
#11715 = ORIENTED_EDGE ( 'NONE', *, *, #19975, .T. ) ;
#11716 = CARTESIAN_POINT ( 'NONE',  ( -8.413264671629002933, 39.99999999999999289, -53.12447868246846383 ) ) ;
#11717 = VERTEX_POINT ( 'NONE', #19991 ) ;
#11718 = CYLINDRICAL_SURFACE ( 'NONE', #9379, 10.00000000000000178 ) ;
#11719 = CARTESIAN_POINT ( 'NONE',  ( -5.863435294608654486E-12, 3.518151346420735669E-15, -50.27768525408826150 ) ) ;
#11720 = VERTEX_POINT ( 'NONE', #2115 ) ;
#11721 = CARTESIAN_POINT ( 'NONE',  ( -35.00000000000058265, 26.00000000000000355, -52.90000000000076597 ) ) ;
#11722 = AXIS2_PLACEMENT_3D ( 'NONE', #5984, #9193, #18010 ) ;
#11723 = CARTESIAN_POINT ( 'NONE',  ( 35.00000000000001421, 0.000000000000000000, 1.540743955509788682E-30 ) ) ;
#11724 = LINE ( 'NONE', #18370, #19159 ) ;
#11725 = EDGE_CURVE ( 'NONE', #14674, #18815, #15084, .T. ) ;
#11726 = CARTESIAN_POINT ( 'NONE',  ( 20.65262896361246803, 28.82759387226735370, -58.26038807538034803 ) ) ;
#11727 = VERTEX_POINT ( 'NONE', #4179 ) ;
#11728 = CIRCLE ( 'NONE', #10612, 31.50000000000001421 ) ;
#11729 = VERTEX_POINT ( 'NONE', #620 ) ;
#11730 = ORIENTED_EDGE ( 'NONE', *, *, #8336, .F. ) ;
#11731 = ORIENTED_EDGE ( 'NONE', *, *, #14414, .F. ) ;
#11732 = DIRECTION ( 'NONE',  ( 6.505213034913038160E-19, 3.903127820947822896E-18, 1.000000000000000000 ) ) ;
#11733 = CARTESIAN_POINT ( 'NONE',  ( -35.00000000000000000, 17.00000000000000000, 2.365113165210053967E-14 ) ) ;
#11734 = ORIENTED_EDGE ( 'NONE', *, *, #17490, .F. ) ;
#11735 = CARTESIAN_POINT ( 'NONE',  ( -28.73472116836718371, 21.94328778841591898, 2.932969818539058693 ) ) ;
#11736 = DIRECTION ( 'NONE',  ( -6.505213034913038160E-19, -3.903127820947822896E-18, -1.000000000000000000 ) ) ;
#11737 = ORIENTED_EDGE ( 'NONE', *, *, #18168, .T. ) ;
#11738 = DIRECTION ( 'NONE',  ( -6.505213034913038160E-19, -3.903127820947822896E-18, -1.000000000000000000 ) ) ;
#11739 = DIRECTION ( 'NONE',  ( -0.000000000000000000, -1.000000000000000000, -0.000000000000000000 ) ) ;
#11740 = EDGE_LOOP ( 'NONE', ( #593, #976, #19303, #19809 ) ) ;
#11741 = CARTESIAN_POINT ( 'NONE',  ( 6.869660410832048036, 39.72568940399584392, -53.24677441048955728 ) ) ;
#11742 = AXIS2_PLACEMENT_3D ( 'NONE', #6698, #11736, #21959 ) ;
#11743 = CARTESIAN_POINT ( 'NONE',  ( 35.00000000000000000, 40.00000000000000000, 4.258610482196280173E-15 ) ) ;
#11744 = CARTESIAN_POINT ( 'NONE',  ( -8.550503583141688679, 23.49231551964756193, -2.999999999999971578 ) ) ;
#11745 = CARTESIAN_POINT ( 'NONE',  ( -19.91015268464082411, 21.95549706463424755, -60.60051340835962463 ) ) ;
#11746 = CIRCLE ( 'NONE', #20159, 36.76383501243555685 ) ;
#11747 = EDGE_CURVE ( 'NONE', #12202, #11599, #11657, .T. ) ;
#11748 = DIRECTION ( 'NONE',  ( -6.505213034913038160E-19, -3.903127820947822896E-18, -1.000000000000000000 ) ) ;
#11749 = ORIENTED_EDGE ( 'NONE', *, *, #13729, .T. ) ;
#11750 = CIRCLE ( 'NONE', #4810, 49.99999999999998579 ) ;
#11751 = ORIENTED_EDGE ( 'NONE', *, *, #13130, .F. ) ;
#11752 = ADVANCED_FACE ( 'NONE', ( #6005 ), #6328, .F. ) ;
#11753 = ORIENTED_EDGE ( 'NONE', *, *, #1305, .T. ) ;
#11754 = CARTESIAN_POINT ( 'NONE',  ( -20.01704759191785499, 20.30656121192005870, 60.62580324355963057 ) ) ;
#11755 = CARTESIAN_POINT ( 'NONE',  ( -4.025500340002458266, 36.54278193890269932, -2.000000000000005329 ) ) ;
#11756 = LINE ( 'NONE', #8439, #9064 ) ;
#11757 = CARTESIAN_POINT ( 'NONE',  ( -12.15643230334918279, 39.99999999999999289, 54.39836425128645914 ) ) ;
#11758 = EDGE_CURVE ( 'NONE', #5648, #3905, #9244, .T. ) ;
#11759 = ORIENTED_EDGE ( 'NONE', *, *, #19972, .F. ) ;
#11760 = CARTESIAN_POINT ( 'NONE',  ( -35.00000000000000000, 10.00000000000000000, 41.00000000000002132 ) ) ;
#11761 = CARTESIAN_POINT ( 'NONE',  ( -6.043799261040989634, 39.99999999999999289, -52.11526435034569715 ) ) ;
#11762 = CARTESIAN_POINT ( 'NONE',  ( -0.8499999999999827693, -5.000000000000000000, 48.11213464397150830 ) ) ;
#11763 = CARTESIAN_POINT ( 'NONE',  ( 11.87329829276352200, 39.99999999999998579, -54.28004929203127205 ) ) ;
#11764 = EDGE_CURVE ( 'NONE', #5453, #19435, #5894, .T. ) ;
#11765 = VERTEX_POINT ( 'NONE', #18150 ) ;
#11766 = DIRECTION ( 'NONE',  ( 6.505213034913038160E-19, 3.903127820947822896E-18, 1.000000000000000000 ) ) ;
#11767 = VERTEX_POINT ( 'NONE', #18265 ) ;
#11768 = DIRECTION ( 'NONE',  ( -0.000000000000000000, 1.000000000000000000, -0.000000000000000000 ) ) ;
#11769 = CARTESIAN_POINT ( 'NONE',  ( -8.479740367039939386, -4.901256658985757575, -50.57596245086818243 ) ) ;
#11770 = DIRECTION ( 'NONE',  ( 6.505213034913038160E-19, 3.903127820947822896E-18, 1.000000000000000000 ) ) ;
#11771 = VERTEX_POINT ( 'NONE', #499 ) ;
#11772 = VERTEX_POINT ( 'NONE', #9107 ) ;
#11773 = CARTESIAN_POINT ( 'NONE',  ( -9.327259741686505734, -2.742977062671840827, 53.40697683846378396 ) ) ;
#11774 = CIRCLE ( 'NONE', #10298, 58.99999999999700862 ) ;
#11775 = DIRECTION ( 'NONE',  ( 1.000000000000000000, 0.000000000000000000, 0.000000000000000000 ) ) ;
#11776 = EDGE_LOOP ( 'NONE', ( #18034, #17973, #18343, #17697 ) ) ;
#11777 = EDGE_CURVE ( 'NONE', #2375, #1150, #2577, .T. ) ;
#11778 = CARTESIAN_POINT ( 'NONE',  ( -89.99999999999701572, -5.000000000000000000, 2.499999999999978684 ) ) ;
#11779 = CARTESIAN_POINT ( 'NONE',  ( 1.079570778443343260, 34.99943186904513936, -38.73482392062543767 ) ) ;
#11780 = DIRECTION ( 'NONE',  ( 6.505213034913038160E-19, 3.903127820947822896E-18, 1.000000000000000000 ) ) ;
#11781 = CARTESIAN_POINT ( 'NONE',  ( -18.56336306567920502, 12.50537704746205847, -60.26262883998990816 ) ) ;
#11782 = LINE ( 'NONE', #20288, #16656 ) ;
#11783 = EDGE_CURVE ( 'NONE', #17600, #10809, #10547, .T. ) ;
#11784 = DIRECTION ( 'NONE',  ( 0.000000000000000000, 1.000000000000000000, 0.000000000000000000 ) ) ;
#11785 = ORIENTED_EDGE ( 'NONE', *, *, #476, .F. ) ;
#11786 = CARTESIAN_POINT ( 'NONE',  ( 13.75658951623322679, 25.99185038947792847, 45.26303799332217181 ) ) ;
#11787 = PRESENTATION_STYLE_ASSIGNMENT (( #6890 ) ) ;
#11788 = CARTESIAN_POINT ( 'NONE',  ( 10.62139969368193881, 0.6004703193305798159, -54.70636795414631592 ) ) ;
#11789 = CARTESIAN_POINT ( 'NONE',  ( 5.999999999999998224, 20.00000000000000000, -5.999999999999999112 ) ) ;
#11790 = VECTOR ( 'NONE', #10173, 999.9999999999998863 ) ;
#11791 = ORIENTED_EDGE ( 'NONE', *, *, #3879, .F. ) ;
#11792 = AXIS2_PLACEMENT_3D ( 'NONE', #19661, #12424, #3740 ) ;
#11793 = CARTESIAN_POINT ( 'NONE',  ( -25.00000000000000000, 20.00000000000000000, 6.487780019669002523E-15 ) ) ;
#11794 = CARTESIAN_POINT ( 'NONE',  ( -5.093313992686365310, -32.09841355226039639, -2.999999999999995559 ) ) ;
#11795 = AXIS2_PLACEMENT_3D ( 'NONE', #5119, #3391, #22656 ) ;
#11796 = EDGE_CURVE ( 'NONE', #21043, #17505, #744, .T. ) ;
#11797 = VERTEX_POINT ( 'NONE', #21706 ) ;
#11798 = ORIENTED_EDGE ( 'NONE', *, *, #14377, .T. ) ;
#11799 = APPLICATION_PROTOCOL_DEFINITION ( 'draft international standard', 'automotive_design', 1998, #20143 ) ;
#11800 = EDGE_CURVE ( 'NONE', #18495, #3688, #16083, .T. ) ;
#11801 = ORIENTED_EDGE ( 'NONE', *, *, #16452, .F. ) ;
#11802 = LINE ( 'NONE', #8485, #18729 ) ;
#11803 = DIRECTION ( 'NONE',  ( 6.505213034913038160E-19, 3.903127820947822896E-18, 1.000000000000000000 ) ) ;
#11804 = AXIS2_PLACEMENT_3D ( 'NONE', #15092, #19937, #6191 ) ;
#11805 = DIRECTION ( 'NONE',  ( -0.000000000000000000, 1.000000000000000000, -0.000000000000000000 ) ) ;
#11806 = AXIS2_PLACEMENT_3D ( 'NONE', #15406, #4784, #1113 ) ;
#11807 = DIRECTION ( 'NONE',  ( -0.000000000000000000, -1.000000000000000000, -0.000000000000000000 ) ) ;
#11808 = CYLINDRICAL_SURFACE ( 'NONE', #22303, 2.500000000000002220 ) ;
#11809 = ORIENTED_EDGE ( 'NONE', *, *, #3177, .T. ) ;
#11810 = DIRECTION ( 'NONE',  ( -0.000000000000000000, -1.000000000000000000, -0.000000000000000000 ) ) ;
#11811 = DIRECTION ( 'NONE',  ( -6.505213034913038160E-19, -3.903127820947822896E-18, -1.000000000000000000 ) ) ;
#11812 = ORIENTED_EDGE ( 'NONE', *, *, #20217, .T. ) ;
#11813 = CARTESIAN_POINT ( 'NONE',  ( 47.83731665821558465, 10.00000000000000000, 38.93845529828710283 ) ) ;
#11814 = AXIS2_PLACEMENT_3D ( 'NONE', #16279, #5868, #4149 ) ;
#11815 = CARTESIAN_POINT ( 'NONE',  ( 32.14641817400198676, 18.83615802559776498, -7.000000000000006217 ) ) ;
#11816 = DIRECTION ( 'NONE',  ( -0.000000000000000000, 1.000000000000000000, -0.000000000000000000 ) ) ;
#11817 = DIRECTION ( 'NONE',  ( 1.000000000000000000, 0.000000000000000000, 0.000000000000000000 ) ) ;
#11818 = ORIENTED_EDGE ( 'NONE', *, *, #10152, .T. ) ;
#11819 = DIRECTION ( 'NONE',  ( -0.000000000000000000, 1.000000000000000000, -0.000000000000000000 ) ) ;
#11820 = ORIENTED_EDGE ( 'NONE', *, *, #14998, .T. ) ;
#11821 = DIRECTION ( 'NONE',  ( 0.000000000000000000, 0.000000000000000000, 1.000000000000000000 ) ) ;
#11822 = CARTESIAN_POINT ( 'NONE',  ( -13.31210290807011276, 38.06413856043590727, 55.94798518139002397 ) ) ;
#11823 = ORIENTED_EDGE ( 'NONE', *, *, #16254, .T. ) ;
#11824 = CARTESIAN_POINT ( 'NONE',  ( -28.52469787935786982, 10.00000000000000000, -4.095854054471906203 ) ) ;
#11825 = CARTESIAN_POINT ( 'NONE',  ( 35.00000000000000000, 7.000000000000000000, 2.365113165210053967E-14 ) ) ;
#11826 = DIRECTION ( 'NONE',  ( -1.000000000000000000, -1.208970125616060717E-17, 0.000000000000000000 ) ) ;
#11827 = B_SPLINE_SURFACE_WITH_KNOTS ( 'NONE', 1, 3, ( 
 ( #15520, #13914, #6719, #15640, #20931, #19666 ),
 ( #7628, #14485, #4195, #7396, #14604, #18042 ) ),
 .UNSPECIFIED., .F., .F., .F.,
 ( 2, 2 ),
 ( 4, 2, 4 ),
 ( 0.000000000000000000, 1.000000000000000000 ),
 ( 0.000000000000000000, 0.001214050925800259527, 0.002428101851600519053 ),
 .UNSPECIFIED. ) ;
#11828 = CARTESIAN_POINT ( 'NONE',  ( 21.60519577075306685, 26.10363331747821647, -58.48615516158968575 ) ) ;
#11829 = EDGE_CURVE ( 'NONE', #11530, #14814, #6691, .T. ) ;
#11830 = CIRCLE ( 'NONE', #8545, 36.76383501243555685 ) ;
#11831 = CIRCLE ( 'NONE', #9997, 4.000000000000000000 ) ;
#11832 = ORIENTED_EDGE ( 'NONE', *, *, #10845, .T. ) ;
#11833 = EDGE_LOOP ( 'NONE', ( #5993, #13240 ) ) ;
#11834 = VERTEX_POINT ( 'NONE', #15030 ) ;
#11835 = EDGE_CURVE ( 'NONE', #13942, #17988, #12177, .T. ) ;
#11836 = EDGE_CURVE ( 'NONE', #7707, #4584, #18761, .T. ) ;
#11837 = ADVANCED_FACE ( 'NONE', ( #11382 ), #19499, .T. ) ;
#11838 = ORIENTED_EDGE ( 'NONE', *, *, #10822, .F. ) ;
#11839 = FACE_OUTER_BOUND ( 'NONE', #8493, .T. ) ;
#11840 = CARTESIAN_POINT ( 'NONE',  ( -42.50000000000000711, -12.00000000000000000, 47.50000000000000711 ) ) ;
#11841 = AXIS2_PLACEMENT_3D ( 'NONE', #14819, #14710, #21720 ) ;
#11842 = VERTEX_POINT ( 'NONE', #14805 ) ;
#11843 = CARTESIAN_POINT ( 'NONE',  ( 15.99999999999997335, 20.00000000000000355, -102.0000000000000142 ) ) ;
#11844 = CARTESIAN_POINT ( 'NONE',  ( -5.961618526223441350, -3.061744126952760325, -51.29856354178470212 ) ) ;
#11845 = ORIENTED_EDGE ( 'NONE', *, *, #10811, .F. ) ;
#11846 = FACE_OUTER_BOUND ( 'NONE', #14644, .T. ) ;
#11847 = DIRECTION ( 'NONE',  ( 0.000000000000000000, 1.000000000000000000, 0.000000000000000000 ) ) ;
#11848 = VECTOR ( 'NONE', #12075, 1000.000000000000000 ) ;
#11849 = ORIENTED_EDGE ( 'NONE', *, *, #21699, .T. ) ;
#11850 = CARTESIAN_POINT ( 'NONE',  ( -1.387778780781445518E-14, 20.00000000000000355, 102.0000000000000142 ) ) ;
#11851 = ADVANCED_FACE ( 'NONE', ( #8072 ), #20972, .F. ) ;
#11852 = CIRCLE ( 'NONE', #4909, 19.11328065563150957 ) ;
#11853 = LINE ( 'NONE', #13665, #10898 ) ;
#11854 = DIRECTION ( 'NONE',  ( -0.000000000000000000, 1.000000000000000000, -0.000000000000000000 ) ) ;
#11855 = FACE_OUTER_BOUND ( 'NONE', #18537, .T. ) ;
#11856 = CIRCLE ( 'NONE', #9288, 34.90673715956759082 ) ;
#11857 = CARTESIAN_POINT ( 'NONE',  ( 11.68090480754629112, 3.765577839755377187, -57.90797000640139913 ) ) ;
#11858 = CONICAL_SURFACE ( 'NONE', #4203, 18.00000000000000000, 0.7853981633974466137 ) ;
#11859 = ORIENTED_EDGE ( 'NONE', *, *, #20183, .F. ) ;
#11860 = ORIENTED_EDGE ( 'NONE', *, *, #19592, .F. ) ;
#11861 = ORIENTED_EDGE ( 'NONE', *, *, #9583, .T. ) ;
#11862 =( GEOMETRIC_REPRESENTATION_CONTEXT ( 3 ) GLOBAL_UNCERTAINTY_ASSIGNED_CONTEXT ( ( #16516 ) ) GLOBAL_UNIT_ASSIGNED_CONTEXT ( ( #20740, #1488, #8473 ) ) REPRESENTATION_CONTEXT ( 'NONE', 'WORKASPACE' ) );
#11863 = ORIENTED_EDGE ( 'NONE', *, *, #12254, .F. ) ;
#11864 = DIRECTION ( 'NONE',  ( 0.000000000000000000, 0.000000000000000000, 1.000000000000000000 ) ) ;
#11865 = CARTESIAN_POINT ( 'NONE',  ( 35.00000000000000000, 17.00000000000000000, 17.00000000000002487 ) ) ;
#11866 = CARTESIAN_POINT ( 'NONE',  ( 0.5386985600499774041, 39.99828252980264409, -49.14867219490655259 ) ) ;
#11867 = CARTESIAN_POINT ( 'NONE',  ( -16.07406985629802421, 8.092854060485290546, -59.53272467997609141 ) ) ;
#11868 = CARTESIAN_POINT ( 'NONE',  ( -11.13570271988771232, 40.00000000000000000, 54.01634158485468618 ) ) ;
#11869 = EDGE_CURVE ( 'NONE', #13841, #17930, #8874, .T. ) ;
#11870 = EDGE_CURVE ( 'NONE', #16838, #8887, #7834, .T. ) ;
#11871 = EDGE_LOOP ( 'NONE', ( #13585, #18156, #15200, #340 ) ) ;
#11872 = VECTOR ( 'NONE', #8453, 999.9999999999998863 ) ;
#11873 = CARTESIAN_POINT ( 'NONE',  ( -26.79308242454879618, -16.56444186175107092, -7.000000000000006217 ) ) ;
#11874 = CARTESIAN_POINT ( 'NONE',  ( -8.448970479837855763, 40.00000000000000000, -53.13698760634334661 ) ) ;
#11875 = LINE ( 'NONE', #20485, #14540 ) ;
#11876 = FACE_OUTER_BOUND ( 'NONE', #2122, .T. ) ;
#11877 = ORIENTED_EDGE ( 'NONE', *, *, #10719, .T. ) ;
#11878 = ADVANCED_FACE ( 'NONE', ( #18830 ), #20105, .F. ) ;
#11879 = CARTESIAN_POINT ( 'NONE',  ( 29.33526866242100439, -22.15900668633777215, -2.800654218530429507 ) ) ;
#11880 = EDGE_LOOP ( 'NONE', ( #8293, #21204 ) ) ;
#11881 = CARTESIAN_POINT ( 'NONE',  ( 3.330669073875469621E-13, -1.110223024625156540E-13, -2.999999999999971578 ) ) ;
#11882 = CARTESIAN_POINT ( 'NONE',  ( -12.99999999999980282, -2.516660498395516310, 100.0000000000000000 ) ) ;
#11883 = CARTESIAN_POINT ( 'NONE',  ( -34.99999999999999289, 1.000000000000044187, -3.012171160963566127E-14 ) ) ;
#11884 = AXIS2_PLACEMENT_3D ( 'NONE', #3891, #9152, #2514 ) ;
#11885 = ORIENTED_EDGE ( 'NONE', *, *, #9046, .T. ) ;
#11886 = AXIS2_PLACEMENT_3D ( 'NONE', #14946, #11748, #20574 ) ;
#11887 = VERTEX_POINT ( 'NONE', #7956 ) ;
#11888 = AXIS2_PLACEMENT_3D ( 'NONE', #13525, #20203, #18476 ) ;
#11889 = CARTESIAN_POINT ( 'NONE',  ( -5.786532357731522858, -4.768624102719487112, 49.22393831245486950 ) ) ;
#11890 = ADVANCED_FACE ( 'NONE', ( #11502 ), #4638, .F. ) ;
#11891 = CARTESIAN_POINT ( 'NONE',  ( 14.76298474240547698, 28.95348479018558407, 2.999999999999995559 ) ) ;
#11892 = ORIENTED_EDGE ( 'NONE', *, *, #1051, .T. ) ;
#11893 = CARTESIAN_POINT ( 'NONE',  ( 14.99999999999998579, 20.00000000000000000, 45.82575694955838230 ) ) ;
#11894 = CARTESIAN_POINT ( 'NONE',  ( -28.06260833510291874, 14.30873905802329560, -2.999999999999981792 ) ) ;
#11895 = DIRECTION ( 'NONE',  ( 0.000000000000000000, 0.000000000000000000, 1.000000000000000000 ) ) ;
#11896 = CIRCLE ( 'NONE', #21421, 25.00000000000000711 ) ;
#11897 = CARTESIAN_POINT ( 'NONE',  ( -19.67606655124792780, 9.154757266468241284, -58.01240525280853433 ) ) ;
#11898 = CARTESIAN_POINT ( 'NONE',  ( -7.471700997414055578, 39.63178059879609805, 53.58785626114602252 ) ) ;
#11899 = CIRCLE ( 'NONE', #17756, 0.9999999999999974465 ) ;
#11900 = DIRECTION ( 'NONE',  ( 0.000000000000000000, 0.000000000000000000, 1.000000000000000000 ) ) ;
#11901 = ORIENTED_EDGE ( 'NONE', *, *, #21397, .T. ) ;
#11902 = DIRECTION ( 'NONE',  ( 0.000000000000000000, 0.000000000000000000, -1.000000000000000000 ) ) ;
#11903 = DIRECTION ( 'NONE',  ( -0.000000000000000000, -0.000000000000000000, -1.000000000000000000 ) ) ;
#11904 = CARTESIAN_POINT ( 'NONE',  ( -35.00000000000000000, 10.00000000000000000, 2.365113165210053967E-14 ) ) ;
#11905 = DIRECTION ( 'NONE',  ( 0.000000000000000000, 0.000000000000000000, 1.000000000000000000 ) ) ;
#11906 = AXIS2_PLACEMENT_3D ( 'NONE', #11656, #664, #4218 ) ;
#11907 = ORIENTED_EDGE ( 'NONE', *, *, #431, .T. ) ;
#11908 = DIRECTION ( 'NONE',  ( -1.000000000000000000, -1.208970125616060101E-17, 6.505213034913038160E-19 ) ) ;
#11909 = CARTESIAN_POINT ( 'NONE',  ( 21.00948735876886886, 24.79619811426206510, -2.999999999999971578 ) ) ;
#11910 = CARTESIAN_POINT ( 'NONE',  ( 2.109039589833486161, 5.113963322222096153, 38.90259428073981240 ) ) ;
#11911 = EDGE_CURVE ( 'NONE', #18993, #17804, #4144, .T. ) ;
#11912 = AXIS2_PLACEMENT_3D ( 'NONE', #15066, #11423, #999 ) ;
#11913 = EDGE_LOOP ( 'NONE', ( #1775, #11276, #4676, #20981 ) ) ;
#11914 = AXIS2_PLACEMENT_3D ( 'NONE', #19785, #9003, #15983 ) ;
#11915 = ADVANCED_FACE ( 'NONE', ( #18611 ), #18486, .F. ) ;
#11916 = AXIS2_PLACEMENT_3D ( 'NONE', #5218, #8766, #2107 ) ;
#11917 = EDGE_CURVE ( 'NONE', #2015, #5630, #16654, .T. ) ;
#11918 = SHAPE_DEFINITION_REPRESENTATION ( #7085, #15726 ) ;
#11919 = EDGE_LOOP ( 'NONE', ( #20091, #15086, #17160, #12729 ) ) ;
#11920 = CARTESIAN_POINT ( 'NONE',  ( 1.387778780781445676E-13, -22.00000000000021316, 3.000000000000002665 ) ) ;
#11921 = AXIS2_PLACEMENT_3D ( 'NONE', #16713, #7772, #21647 ) ;
#11922 = DIRECTION ( 'NONE',  ( -1.000000000000000000, 1.061893299983986855E-14, 0.000000000000000000 ) ) ;
#11923 = DIRECTION ( 'NONE',  ( 1.296372316667914327E-16, 1.000000000000000000, -0.000000000000000000 ) ) ;
#11924 = DIRECTION ( 'NONE',  ( -1.000000000000000000, 1.734723475976807834E-16, 0.000000000000000000 ) ) ;
#11925 = DIRECTION ( 'NONE',  ( -0.000000000000000000, -0.000000000000000000, -1.000000000000000000 ) ) ;
#11926 = ORIENTED_EDGE ( 'NONE', *, *, #15758, .F. ) ;
#11927 = CARTESIAN_POINT ( 'NONE',  ( 2.775557561562891351E-14, 2.775557561562891351E-14, 5.750000000000001776 ) ) ;
#11928 = CARTESIAN_POINT ( 'NONE',  ( -11.15511648636534048, 39.11609166919075875, 55.07420106209026756 ) ) ;
#11929 = ORIENTED_EDGE ( 'NONE', *, *, #789, .T. ) ;
#11930 = DIRECTION ( 'NONE',  ( 1.000000000000000000, 0.000000000000000000, 0.000000000000000000 ) ) ;
#11931 = CARTESIAN_POINT ( 'NONE',  ( -42.50000000000000711, -9.600000000000001421, -45.40000000000000568 ) ) ;
#11932 = CARTESIAN_POINT ( 'NONE',  ( 34.00000000000000000, -6.180736333215569367, 0.000000000000000000 ) ) ;
#11933 = FACE_OUTER_BOUND ( 'NONE', #15148, .T. ) ;
#11934 = ORIENTED_EDGE ( 'NONE', *, *, #19285, .T. ) ;
#11935 = CARTESIAN_POINT ( 'NONE',  ( 14.69988787053502222, 23.08500126984897349, -45.69379240540676079 ) ) ;
#11936 = EDGE_CURVE ( 'NONE', #19954, #9032, #11724, .T. ) ;
#11937 = ORIENTED_EDGE ( 'NONE', *, *, #4182, .F. ) ;
#11938 = CARTESIAN_POINT ( 'NONE',  ( 5.004946378181853284, 0.5943096879531043486, -54.03132084814315306 ) ) ;
#11939 = AXIS2_PLACEMENT_3D ( 'NONE', #18596, #1625, #3119 ) ;
#11940 = VECTOR ( 'NONE', #10599, 1000.000000000000000 ) ;
#11941 = CARTESIAN_POINT ( 'NONE',  ( -22.32664865868314763, 17.89874346835047092, 58.64628984943162493 ) ) ;
#11942 = CIRCLE ( 'NONE', #19637, 2.500000000000002220 ) ;
#11943 = VECTOR ( 'NONE', #21300, 1000.000000000000000 ) ;
#11944 = ORIENTED_EDGE ( 'NONE', *, *, #14871, .F. ) ;
#11945 = DIRECTION ( 'NONE',  ( 1.000000000000000000, 0.000000000000000000, 0.000000000000000000 ) ) ;
#11946 = DIRECTION ( 'NONE',  ( -0.000000000000000000, 1.000000000000000000, -0.000000000000000000 ) ) ;
#11947 = CYLINDRICAL_SURFACE ( 'NONE', #7072, 19.00000000000000355 ) ;
#11948 = EDGE_CURVE ( 'NONE', #9581, #7786, #7434, .T. ) ;
#11949 = AXIS2_PLACEMENT_3D ( 'NONE', #4549, #18177, #16680 ) ;
#11950 = CARTESIAN_POINT ( 'NONE',  ( 15.00671337312779663, 3.288799316213545154, -56.57538198732802215 ) ) ;
#11951 = ORIENTED_EDGE ( 'NONE', *, *, #6852, .T. ) ;
#11952 = ORIENTED_EDGE ( 'NONE', *, *, #18575, .F. ) ;
#11953 = EDGE_LOOP ( 'NONE', ( #7349, #2289, #7424, #9485 ) ) ;
#11954 = AXIS2_PLACEMENT_3D ( 'NONE', #5376, #10734, #3438 ) ;
#11955 = ORIENTED_EDGE ( 'NONE', *, *, #8922, .T. ) ;
#11956 = LINE ( 'NONE', #18956, #3736 ) ;
#11957 = CARTESIAN_POINT ( 'NONE',  ( 21.80163436544120970, 14.71892543950345100, 58.53048140122282916 ) ) ;
#11958 = DIRECTION ( 'NONE',  ( 6.505213034913038160E-19, 3.903127820947822896E-18, 1.000000000000000000 ) ) ;
#11959 = ORIENTED_EDGE ( 'NONE', *, *, #7534, .T. ) ;
#11960 = FACE_BOUND ( 'NONE', #19168, .T. ) ;
#11961 = CARTESIAN_POINT ( 'NONE',  ( 1.110223024625156540E-13, -27.99999999999999645, -2.999999999999971578 ) ) ;
#11962 = ORIENTED_EDGE ( 'NONE', *, *, #5855, .T. ) ;
#11963 = CARTESIAN_POINT ( 'NONE',  ( 6.696867368503558448E-15, 40.00000000000000000, 48.73397172404481381 ) ) ;
#11964 = AXIS2_PLACEMENT_3D ( 'NONE', #4110, #2387, #5828 ) ;
#11965 = CARTESIAN_POINT ( 'NONE',  ( 35.00000000000000000, 39.00000000000000711, 4.258610482196280173E-15 ) ) ;
#11966 = EDGE_CURVE ( 'NONE', #20409, #1875, #9667, .T. ) ;
#11967 = CARTESIAN_POINT ( 'NONE',  ( -42.50000000000000000, 7.000000000000000000, 44.99999999999999289 ) ) ;
#11968 = VERTEX_POINT ( 'NONE', #13194 ) ;
#11969 = DIRECTION ( 'NONE',  ( 0.000000000000000000, 0.000000000000000000, 1.000000000000000000 ) ) ;
#11970 = CARTESIAN_POINT ( 'NONE',  ( -15.99999999999994493, 20.00000000000000355, 102.0000000000000142 ) ) ;
#11971 = DIRECTION ( 'NONE',  ( -6.505213034913038160E-19, -3.903127820947822896E-18, -1.000000000000000000 ) ) ;
#11972 = CARTESIAN_POINT ( 'NONE',  ( -3.658199643160841230, 39.91812894417287083, 51.36232514819826633 ) ) ;
#11973 = AXIS2_PLACEMENT_3D ( 'NONE', #5399, #7109, #578 ) ;
#11974 = CARTESIAN_POINT ( 'NONE',  ( -10.39230484541304911, 1.500000000000005773, -6.000000000000371259 ) ) ;
#11975 = ADVANCED_FACE ( 'NONE', ( #20216 ), #4520, .F. ) ;
#11976 = CIRCLE ( 'NONE', #22224, 6.499999999999999112 ) ;
#11977 = DIRECTION ( 'NONE',  ( -1.000000000000000000, -1.208970125616060101E-17, 6.505213034913038160E-19 ) ) ;
#11978 = VERTEX_POINT ( 'NONE', #1083 ) ;
#11979 = EDGE_LOOP ( 'NONE', ( #10810, #5762, #16428, #11069, #11625, #17874, #2456, #4712, #1117, #13702, #19540, #7793, #11127, #11983 ) ) ;
#11980 = AXIS2_PLACEMENT_3D ( 'NONE', #13083, #9554, #16429 ) ;
#11981 = VECTOR ( 'NONE', #19555, 1000.000000000000000 ) ;
#11982 = ADVANCED_FACE ( 'NONE', ( #6460 ), #3024, .T. ) ;
#11983 = ORIENTED_EDGE ( 'NONE', *, *, #4663, .T. ) ;
#11984 = ORIENTED_EDGE ( 'NONE', *, *, #19694, .F. ) ;
#11985 = CARTESIAN_POINT ( 'NONE',  ( -35.00000000000000000, 25.00000000000000000, 1.387778780781445676E-14 ) ) ;
#11986 = DIRECTION ( 'NONE',  ( 6.505213034913038160E-19, 3.903127820947822896E-18, 1.000000000000000000 ) ) ;
#11987 = AXIS2_PLACEMENT_3D ( 'NONE', #605, #16412, #21583 ) ;
#11988 = AXIS2_PLACEMENT_3D ( 'NONE', #17884, #8940, #21100 ) ;
#11989 = EDGE_CURVE ( 'NONE', #15903, #13430, #7034, .T. ) ;
#11990 = DIRECTION ( 'NONE',  ( 6.505213034913038160E-19, 3.903127820947822896E-18, 1.000000000000000000 ) ) ;
#11991 = CARTESIAN_POINT ( 'NONE',  ( -10.75185716664304358, 40.00000000000000000, 53.88525272612042727 ) ) ;
#11992 = ADVANCED_FACE ( 'NONE', ( #15817 ), #11947, .T. ) ;
#11993 = ORIENTED_EDGE ( 'NONE', *, *, #6644, .F. ) ;
#11994 = CARTESIAN_POINT ( 'NONE',  ( -34.99999999999999289, 2.142135623730931471, 60.00000000000001421 ) ) ;
#11995 = CARTESIAN_POINT ( 'NONE',  ( -5.890136611214193074, 40.00000000000000711, -52.04311946512136444 ) ) ;
#11996 = DIRECTION ( 'NONE',  ( 6.505213034913038160E-19, 3.903127820947822896E-18, 1.000000000000000000 ) ) ;
#11997 = B_SPLINE_CURVE_WITH_KNOTS ( 'NONE', 3,
 ( #8003, #6387, #19805, #663, #13012, #4566, #11543, #18533, #2504, #21748 ),
 .UNSPECIFIED., .F., .F.,
 ( 4, 2, 2, 2, 4 ),
 ( 0.000000000000000000, 0.002975785561746833834, 0.005951571123493670269, 0.008927356685240507572, 0.01190314224698734054 ),
 .UNSPECIFIED. ) ;
#11998 = CYLINDRICAL_SURFACE ( 'NONE', #14079, 6.499999999999999112 ) ;
#11999 = ORIENTED_EDGE ( 'NONE', *, *, #8128, .F. ) ;
#12000 = CARTESIAN_POINT ( 'NONE',  ( 8.657955327455969297, 40.00000000000002132, -53.21471618982314311 ) ) ;
#12001 = VECTOR ( 'NONE', #28, 1000.000000000000000 ) ;
#12002 = CARTESIAN_POINT ( 'NONE',  ( 2.999999999999997780, 22.00000000000000000, 8.485281374238567764 ) ) ;
#12003 = EDGE_LOOP ( 'NONE', ( #18763, #9635, #18045, #17071 ) ) ;
#12004 = AXIS2_PLACEMENT_3D ( 'NONE', #18500, #10008, #20228 ) ;
#12005 = AXIS2_PLACEMENT_3D ( 'NONE', #20397, #14870, #22231 ) ;
#12006 = DIRECTION ( 'NONE',  ( -1.000000000000000000, 0.000000000000000000, 0.000000000000000000 ) ) ;
#12007 = CARTESIAN_POINT ( 'NONE',  ( -21.05198877411799785, 30.13956425491218383, -1.999999999999977573 ) ) ;
#12008 = AXIS2_PLACEMENT_3D ( 'NONE', #16211, #10826, #15865 ) ;
#12009 = CARTESIAN_POINT ( 'NONE',  ( 0.000000000000000000, 40.00000000000000000, 9.068199145005368464E-15 ) ) ;
#12010 = CIRCLE ( 'NONE', #14560, 1.000000000000000888 ) ;
#12011 = EDGE_CURVE ( 'NONE', #15997, #13383, #19892, .T. ) ;
#12012 = ORIENTED_EDGE ( 'NONE', *, *, #15136, .T. ) ;
#12013 = EDGE_CURVE ( 'NONE', #18007, #21600, #10220, .T. ) ;
#12014 = ORIENTED_EDGE ( 'NONE', *, *, #22469, .F. ) ;
#12015 = CARTESIAN_POINT ( 'NONE',  ( 1.040180180071618610, -3.147605209281759464, 46.52651510289677361 ) ) ;
#12016 = AXIS2_PLACEMENT_3D ( 'NONE', #17485, #20937, #15411 ) ;
#12017 = EDGE_CURVE ( 'NONE', #14229, #16393, #12198, .T. ) ;
#12018 = CARTESIAN_POINT ( 'NONE',  ( -34.99999999999999289, 2.142135623730931471, 50.00000000000001421 ) ) ;
#12019 = EDGE_LOOP ( 'NONE', ( #10989, #21452 ) ) ;
#12020 = AXIS2_PLACEMENT_3D ( 'NONE', #22172, #20564, #11398 ) ;
#12021 = CARTESIAN_POINT ( 'NONE',  ( 12.48541242016034403, 11.67824612544539420, 44.64471390988170896 ) ) ;
#12022 = LINE ( 'NONE', #8357, #10685 ) ;
#12023 = FACE_OUTER_BOUND ( 'NONE', #8233, .T. ) ;
#12024 = CARTESIAN_POINT ( 'NONE',  ( -19.88513910325156431, 17.69449494136243572, -58.11726460477454737 ) ) ;
#12025 = VECTOR ( 'NONE', #8408, 1000.000000000000000 ) ;
#12026 = CARTESIAN_POINT ( 'NONE',  ( 13.85640646055118808, -25.00000000000000000, 7.999999999999710454 ) ) ;
#12027 = ORIENTED_EDGE ( 'NONE', *, *, #21989, .T. ) ;
#12028 = DIRECTION ( 'NONE',  ( -0.000000000000000000, -1.000000000000000000, -0.000000000000000000 ) ) ;
#12029 = FILL_AREA_STYLE ('',( #5049 ) ) ;
#12030 = FACE_BOUND ( 'NONE', #3589, .T. ) ;
#12031 = FACE_OUTER_BOUND ( 'NONE', #22474, .T. ) ;
#12032 = ORIENTED_EDGE ( 'NONE', *, *, #4252, .T. ) ;
#12033 = AXIS2_PLACEMENT_3D ( 'NONE', #13464, #6498, #22549 ) ;
#12034 = CARTESIAN_POINT ( 'NONE',  ( -12.31876324338254669, -30.07487443287981677, -6.999999999999950262 ) ) ;
#12035 = FACE_OUTER_BOUND ( 'NONE', #1109, .T. ) ;
#12036 = AXIS2_PLACEMENT_3D ( 'NONE', #15699, #15581, #8829 ) ;
#12037 = EDGE_CURVE ( 'NONE', #4151, #20949, #15208, .T. ) ;
#12038 = CARTESIAN_POINT ( 'NONE',  ( -22.05221796475962392, 24.18157222985895061, -58.58672997744003652 ) ) ;
#12039 = ORIENTED_EDGE ( 'NONE', *, *, #17951, .T. ) ;
#12040 = EDGE_CURVE ( 'NONE', #21119, #8612, #6345, .T. ) ;
#12041 = APPLICATION_PROTOCOL_DEFINITION ( 'draft international standard', 'automotive_design', 1998, #14261 ) ;
#12042 = VERTEX_POINT ( 'NONE', #13877 ) ;
#12043 = DIRECTION ( 'NONE',  ( -1.000000000000000000, 0.000000000000000000, 0.000000000000000000 ) ) ;
#12044 = DIRECTION ( 'NONE',  ( -0.000000000000000000, -1.000000000000000000, -0.000000000000000000 ) ) ;
#12045 = CIRCLE ( 'NONE', #14593, 25.00000000000000000 ) ;
#12046 = FACE_OUTER_BOUND ( 'NONE', #15531, .T. ) ;
#12047 = ORIENTED_EDGE ( 'NONE', *, *, #19895, .T. ) ;
#12048 = CARTESIAN_POINT ( 'NONE',  ( -1.387778780781445518E-14, 20.00000000000000355, -102.9999999999999716 ) ) ;
#12049 = CARTESIAN_POINT ( 'NONE',  ( -12.24744603030440970, 40.00000000000000000, 54.43639671998951002 ) ) ;
#12050 = ORIENTED_EDGE ( 'NONE', *, *, #19732, .T. ) ;
#12051 = LINE ( 'NONE', #8606, #8313 ) ;
#12052 = ADVANCED_FACE ( 'NONE', ( #14087 ), #3595, .F. ) ;
#12053 = FACE_OUTER_BOUND ( 'NONE', #16571, .T. ) ;
#12054 = CARTESIAN_POINT ( 'NONE',  ( 0.000000000000000000, 0.000000000000000000, -8.999999999999998224 ) ) ;
#12055 = CARTESIAN_POINT ( 'NONE',  ( 5.400043148885023570, 39.81718169346567748, 52.45350586640867618 ) ) ;
#12056 = CARTESIAN_POINT ( 'NONE',  ( -2.633052209763709239, 39.95897179397861265, -50.67294425775457967 ) ) ;
#12057 = ORIENTED_EDGE ( 'NONE', *, *, #7731, .T. ) ;
#12058 = LINE ( 'NONE', #4749, #17797 ) ;
#12059 = CARTESIAN_POINT ( 'NONE',  ( -11.86180952234344588, 38.99999999999292299, 55.35904751185378103 ) ) ;
#12060 = ORIENTED_EDGE ( 'NONE', *, *, #20881, .T. ) ;
#12061 = DIRECTION ( 'NONE',  ( 6.505213034913038160E-19, 3.903127820947822896E-18, 1.000000000000000000 ) ) ;
#12062 = EDGE_CURVE ( 'NONE', #312, #11717, #20254, .T. ) ;
#12063 =( BOUNDED_SURFACE ( )  B_SPLINE_SURFACE ( 3, 2, ( 
 ( #13551, #4870, #6472 ),
 ( #20229, #18501, #20344 ),
 ( #17000, #4651, #11624 ),
 ( #18628, #11844, #1308 ),
 ( #1195, #13437, #2933 ),
 ( #10120, #16896, #18846 ),
 ( #3150, #12080, #10667 ),
 ( #13778, #17674, #1774 ),
 ( #21018, #1984, #1877 ),
 ( #17227, #8758, #3495 ) ),
 .UNSPECIFIED., .F., .F., .F. ) 
 B_SPLINE_SURFACE_WITH_KNOTS ( ( 4, 2, 2, 2, 4 ),
 ( 3, 3 ),
 ( 0.02809317535148383310, 0.03071213539476958312, 0.03333109543805533315, 0.03595005548134108664, 0.03856901552462683319 ),
 ( 0.2389732943673004428, 1.000000000000000000 ),
 .UNSPECIFIED. ) 
 GEOMETRIC_REPRESENTATION_ITEM ( )  RATIONAL_B_SPLINE_SURFACE ( (
 ( 0.9723126933862541454, 0.9420702913958439728, 1.000000000000000000),
 ( 0.9749922925143332808, 0.9476767737753362120, 1.000000000000000000),
 ( 0.9774153414778116167, 0.9527464803504863688, 1.000000000000000000),
 ( 0.9815341666524188824, 0.9613642323581159665, 1.000000000000000000),
 ( 0.9832251939807838959, 0.9649023417791752211, 1.000000000000000000),
 ( 0.9856873122312947988, 0.9700537923984370314, 1.000000000000000000),
 ( 0.9864553338148032147, 0.9716607116685207490, 1.000000000000000000),
 ( 0.9870557760262982372, 0.9729170072999733243, 1.000000000000000000),
 ( 0.9868934176577572881, 0.9725773074833666820, 1.000000000000000000),
 ( 0.9863383242652690175, 0.9714158944602964141, 1.000000000000000000) ) ) 
 REPRESENTATION_ITEM ( '' )  SURFACE ( )  );
#12064 = CYLINDRICAL_SURFACE ( 'NONE', #7526, 39.00000000000000000 ) ;
#12065 = CARTESIAN_POINT ( 'NONE',  ( 24.43377932785621809, -26.64693883069189795, -2.933296326616325889 ) ) ;
#12066 = DIRECTION ( 'NONE',  ( 0.000000000000000000, -0.000000000000000000, -1.000000000000000000 ) ) ;
#12067 = VECTOR ( 'NONE', #8097, 1000.000000000000114 ) ;
#12068 = B_SPLINE_CURVE_WITH_KNOTS ( 'NONE', 3,
 ( #907, #11096, #21769, #5842 ),
 .UNSPECIFIED., .F., .F.,
 ( 4, 4 ),
 ( 9.715086407578286637E-07, 0.001929643240672447449 ),
 .UNSPECIFIED. ) ;
#12069 = ORIENTED_EDGE ( 'NONE', *, *, #6055, .F. ) ;
#12070 = VERTEX_POINT ( 'NONE', #15597 ) ;
#12071 = ORIENTED_EDGE ( 'NONE', *, *, #13589, .F. ) ;
#12072 = CARTESIAN_POINT ( 'NONE',  ( 42.50000000000000711, -12.00000000000000000, 47.50000000000000711 ) ) ;
#12073 = VERTEX_POINT ( 'NONE', #17212 ) ;
#12074 = CARTESIAN_POINT ( 'NONE',  ( 30.13956425491259949, 21.05198877411795877, -2.800654218530485018 ) ) ;
#12075 = DIRECTION ( 'NONE',  ( 6.505213034913038160E-19, 3.903127820947822896E-18, 1.000000000000000000 ) ) ;
#12076 = CIRCLE ( 'NONE', #8413, 19.11328065563152379 ) ;
#12077 = CARTESIAN_POINT ( 'NONE',  ( 8.410512267088693150, 40.00000000000000711, -53.12343718209208987 ) ) ;
#12078 = EDGE_LOOP ( 'NONE', ( #19689, #17072, #447, #12802 ) ) ;
#12079 = DIRECTION ( 'NONE',  ( -0.000000000000000000, 1.000000000000000000, -0.000000000000000000 ) ) ;
#12080 = CARTESIAN_POINT ( 'NONE',  ( -2.419767991116313688, -3.149022461034792109, -49.02154318834896429 ) ) ;
#12081 = ORIENTED_EDGE ( 'NONE', *, *, #14436, .F. ) ;
#12082 = EDGE_CURVE ( 'NONE', #20866, #7020, #7124, .T. ) ;
#12083 = CARTESIAN_POINT ( 'NONE',  ( -12.99999999999980282, -2.516660498395516310, 100.0000000000000000 ) ) ;
#12084 = CARTESIAN_POINT ( 'NONE',  ( -35.00000000000000000, 17.00000000000000000, 2.365113165210053967E-14 ) ) ;
#12085 = AXIS2_PLACEMENT_3D ( 'NONE', #18175, #3983, #12659 ) ;
#12086 = CARTESIAN_POINT ( 'NONE',  ( 4.078319513017754971, 34.44279552714540671, 39.58919430873140755 ) ) ;
#12087 = ORIENTED_EDGE ( 'NONE', *, *, #7613, .T. ) ;
#12088 = CARTESIAN_POINT ( 'NONE',  ( -9.576564013118904484, 26.31139338200535960, -4.999999999999948486 ) ) ;
#12089 = DIRECTION ( 'NONE',  ( 0.000000000000000000, 1.000000000000000000, -0.000000000000000000 ) ) ;
#12090 = ADVANCED_FACE ( 'NONE', ( #5306 ), #11094, .T. ) ;
#12091 = DIRECTION ( 'NONE',  ( -0.000000000000000000, -1.000000000000000000, -0.000000000000000000 ) ) ;
#12092 = DIRECTION ( 'NONE',  ( 6.505213034913038160E-19, 3.903127820947822896E-18, 1.000000000000000000 ) ) ;
#12093 = CARTESIAN_POINT ( 'NONE',  ( -35.00000000000000000, 22.00000000000000711, 2.255140518769849223E-14 ) ) ;
#12094 = ORIENTED_EDGE ( 'NONE', *, *, #5944, .T. ) ;
#12095 = ORIENTED_EDGE ( 'NONE', *, *, #17750, .F. ) ;
#12096 = EDGE_CURVE ( 'NONE', #4210, #7013, #5979, .T. ) ;
#12097 = EDGE_LOOP ( 'NONE', ( #17356, #13161, #5899, #20891 ) ) ;
#12098 = ORIENTED_EDGE ( 'NONE', *, *, #14031, .T. ) ;
#12099 = CARTESIAN_POINT ( 'NONE',  ( 35.00000000000000000, -9.000000000000001776, -18.00000000000000000 ) ) ;
#12100 = CARTESIAN_POINT ( 'NONE',  ( -12.00937115242649256, -34.74700806321106938, -2.800654218530485018 ) ) ;
#12101 = CARTESIAN_POINT ( 'NONE',  ( -19.05255888325750746, 10.99999999999970512, 3.000000000000006217 ) ) ;
#12102 = CARTESIAN_POINT ( 'NONE',  ( 3.655628638892812088, 39.91824801334192330, 51.36063814675617323 ) ) ;
#12103 = EDGE_CURVE ( 'NONE', #12952, #15024, #17436, .T. ) ;
#12104 = CIRCLE ( 'NONE', #2229, 16.49999999999999645 ) ;
#12105 = ORIENTED_EDGE ( 'NONE', *, *, #15621, .T. ) ;
#12106 = DIRECTION ( 'NONE',  ( 0.000000000000000000, 0.000000000000000000, -1.000000000000000000 ) ) ;
#12107 = DIRECTION ( 'NONE',  ( 6.505213034913038160E-19, 3.903127820947822896E-18, 1.000000000000000000 ) ) ;
#12108 = DIRECTION ( 'NONE',  ( -1.000000000000000000, -1.208970125616063798E-17, 0.000000000000000000 ) ) ;
#12109 = CARTESIAN_POINT ( 'NONE',  ( 9.689843208404399277, 39.33333333333334281, -54.54983754392740281 ) ) ;
#12110 = ORIENTED_EDGE ( 'NONE', *, *, #10724, .T. ) ;
#12111 = ADVANCED_FACE ( 'NONE', ( #1756, #19288 ), #19058, .F. ) ;
#12112 = SURFACE_STYLE_FILL_AREA ( #21051 ) ;
#12113 = VERTEX_POINT ( 'NONE', #8742 ) ;
#12114 = CARTESIAN_POINT ( 'NONE',  ( -8.620004424458363346, 38.06588350694461553, 54.65497187427080661 ) ) ;
#12115 = CARTESIAN_POINT ( 'NONE',  ( 35.00000000000001421, 1.000000000000044187, 1.540743955509788682E-30 ) ) ;
#12116 = CARTESIAN_POINT ( 'NONE',  ( -17.66631876130905709, 31.41173278719225337, -2.999999999999971578 ) ) ;
#12117 = EDGE_CURVE ( 'NONE', #7482, #21816, #477, .T. ) ;
#12118 = VERTEX_POINT ( 'NONE', #128 ) ;
#12119 = ORIENTED_EDGE ( 'NONE', *, *, #20577, .F. ) ;
#12120 = EDGE_CURVE ( 'NONE', #17695, #6172, #21110, .T. ) ;
#12121 = EDGE_LOOP ( 'NONE', ( #2928, #19034, #2664, #20414 ) ) ;
#12122 = LINE ( 'NONE', #1821, #146 ) ;
#12123 = DIRECTION ( 'NONE',  ( -0.000000000000000000, -0.000000000000000000, -1.000000000000000000 ) ) ;
#12124 = EDGE_CURVE ( 'NONE', #4381, #13358, #21728, .T. ) ;
#12125 = ADVANCED_FACE ( 'NONE', ( #1969 ), #18407, .T. ) ;
#12126 = ORIENTED_EDGE ( 'NONE', *, *, #14203, .T. ) ;
#12127 = CARTESIAN_POINT ( 'NONE',  ( 35.00000000000000000, 6.999999999999999112, -40.99999999999997868 ) ) ;
#12128 = VECTOR ( 'NONE', #13615, 1000.000000000000000 ) ;
#12129 = LINE ( 'NONE', #6635, #9960 ) ;
#12130 = CARTESIAN_POINT ( 'NONE',  ( 10.70799354677379256, -35.16985127952393242, 2.800654218530485018 ) ) ;
#12131 = CARTESIAN_POINT ( 'NONE',  ( -21.16618710811416904, 27.45243199383212485, -58.38369730662816437 ) ) ;
#12132 = EDGE_CURVE ( 'NONE', #478, #2004, #14061, .T. ) ;
#12133 = DIRECTION ( 'NONE',  ( 0.000000000000000000, 0.000000000000000000, 1.000000000000000000 ) ) ;
#12134 = ORIENTED_EDGE ( 'NONE', *, *, #1184, .F. ) ;
#12135 = FACE_OUTER_BOUND ( 'NONE', #15475, .T. ) ;
#12136 = B_SPLINE_CURVE_WITH_KNOTS ( 'NONE', 3,
 ( #16389, #15099, #20739, #17174, #2987, #20403, #2876, #16947, #1037, #11786, #22238, #3093, #9956, #6758, #17061, #8472, #1253, #15440, #15218, #10063, #13720, #20615, #4927, #22462 ),
 .UNSPECIFIED., .F., .F.,
 ( 4, 2, 2, 2, 2, 2, 2, 2, 2, 2, 2, 4 ),
 ( 0.02614117015034102265, 0.02729036340605313360, 0.02843955666176524455, 0.03073794317318946645, 0.03188713642890157740, 0.03303632968461368141, 0.03533471619603791025, 0.03648390945175002120, 0.03763310270746213215, 0.03993148921888635405, 0.04222987573031057595, 0.04452826224173479785 ),
 .UNSPECIFIED. ) ;
#12137 = EDGE_CURVE ( 'NONE', #18451, #767, #22088, .T. ) ;
#12138 = FACE_OUTER_BOUND ( 'NONE', #14781, .T. ) ;
#12139 = DIRECTION ( 'NONE',  ( 0.000000000000000000, 0.000000000000000000, 1.000000000000000000 ) ) ;
#12140 = CARTESIAN_POINT ( 'NONE',  ( 34.65667543218853552, 4.170748987303296573, -2.999999999999975131 ) ) ;
#12141 = ORIENTED_EDGE ( 'NONE', *, *, #1295, .F. ) ;
#12142 = DIRECTION ( 'NONE',  ( -0.000000000000000000, 1.000000000000000000, -0.000000000000000000 ) ) ;
#12143 = CARTESIAN_POINT ( 'NONE',  ( 1.387778780781445676E-14, -1.000000000000028644, -48.73397172404115452 ) ) ;
#12144 = CONICAL_SURFACE ( 'NONE', #15055, 2.099999999999997868, 1.029744258676652091 ) ;
#12145 = ORIENTED_EDGE ( 'NONE', *, *, #19378, .T. ) ;
#12146 = PRODUCT_CONTEXT ( 'NONE', #84, 'mechanical' ) ;
#12147 = EDGE_LOOP ( 'NONE', ( #9092, #13483, #22181, #19222 ) ) ;
#12148 = CARTESIAN_POINT ( 'NONE',  ( -35.00000000000058265, 40.00000000000000711, -57.52500000000076597 ) ) ;
#12149 = CARTESIAN_POINT ( 'NONE',  ( -24.41514043009200563, -26.50842683089765828, 3.000000000000002665 ) ) ;
#12150 = CARTESIAN_POINT ( 'NONE',  ( -35.00000000000000000, 13.99999999999999822, -14.99999999999997691 ) ) ;
#12151 = LINE ( 'NONE', #2062, #7237 ) ;
#12152 = CARTESIAN_POINT ( 'NONE',  ( 2.602085213965210642E-15, 0.6398376396478597794, 0.000000000000000000 ) ) ;
#12153 = VERTEX_POINT ( 'NONE', #3704 ) ;
#12154 = CARTESIAN_POINT ( 'NONE',  ( -42.50000000000000711, -12.00000000000012434, -47.50000000000000000 ) ) ;
#12155 = LINE ( 'NONE', #6780, #8323 ) ;
#12156 = VERTEX_POINT ( 'NONE', #16156 ) ;
#12157 = CARTESIAN_POINT ( 'NONE',  ( 4.025500340002624355, -36.54278193890314697, 2.800654218530485018 ) ) ;
#12158 = EDGE_CURVE ( 'NONE', #21624, #21565, #2314, .T. ) ;
#12159 = CARTESIAN_POINT ( 'NONE',  ( 14.27302218980889315, 2.669631712211250285, -56.31136122552219803 ) ) ;
#12160 = CIRCLE ( 'NONE', #9963, 36.76383501243555685 ) ;
#12161 = CARTESIAN_POINT ( 'NONE',  ( -0.6841746959067307454, -36.75746821813308429, 2.800654218530485018 ) ) ;
#12162 = ADVANCED_FACE ( 'NONE', ( #14435 ), #4524, .T. ) ;
#12163 = DIRECTION ( 'NONE',  ( -1.000000000000000000, -1.208970125616077665E-17, 0.000000000000000000 ) ) ;
#12164 = CARTESIAN_POINT ( 'NONE',  ( -10.39230484541300825, -25.00000000000000000, -6.000000000000442313 ) ) ;
#12165 = ORIENTED_EDGE ( 'NONE', *, *, #16979, .T. ) ;
#12166 = DIRECTION ( 'NONE',  ( -0.000000000000000000, 0.000000000000000000, 1.000000000000000000 ) ) ;
#12167 = DIRECTION ( 'NONE',  ( 0.000000000000000000, 0.000000000000000000, 1.000000000000000000 ) ) ;
#12168 = ORIENTED_EDGE ( 'NONE', *, *, #9555, .T. ) ;
#12169 = DIRECTION ( 'NONE',  ( -1.000000000000000000, 0.000000000000000000, 1.445602896647339163E-16 ) ) ;
#12170 = EDGE_CURVE ( 'NONE', #15875, #6249, #5599, .T. ) ;
#12171 = CARTESIAN_POINT ( 'NONE',  ( -20.36304159388362223, -24.03323817228478276, 3.000000000000023537 ) ) ;
#12172 = CARTESIAN_POINT ( 'NONE',  ( 3.330669073875469621E-13, -1.110223024625156540E-13, -2.999999999999971578 ) ) ;
#12173 = ORIENTED_EDGE ( 'NONE', *, *, #13952, .F. ) ;
#12174 = VECTOR ( 'NONE', #19296, 1000.000000000000000 ) ;
#12175 = ORIENTED_EDGE ( 'NONE', *, *, #8501, .F. ) ;
#12176 = EDGE_LOOP ( 'NONE', ( #45, #22166, #16814, #12178 ) ) ;
#12177 = CIRCLE ( 'NONE', #5241, 36.76383501243555685 ) ;
#12178 = ORIENTED_EDGE ( 'NONE', *, *, #20146, .F. ) ;
#12179 = DIRECTION ( 'NONE',  ( -6.505213034913038160E-19, -3.903127820947822896E-18, -1.000000000000000000 ) ) ;
#12180 = CARTESIAN_POINT ( 'NONE',  ( 16.26546936781294050, 4.421830200407478983, 57.01255691153428984 ) ) ;
#12181 = EDGE_CURVE ( 'NONE', #11321, #5360, #14208, .T. ) ;
#12182 = DIRECTION ( 'NONE',  ( 0.000000000000000000, 0.000000000000000000, 1.000000000000000000 ) ) ;
#12183 = CARTESIAN_POINT ( 'NONE',  ( 8.540030399951877627, 39.99999999999999289, 53.17106804086055405 ) ) ;
#12184 = VERTEX_POINT ( 'NONE', #3807 ) ;
#12185 = DIRECTION ( 'NONE',  ( -1.000000000000000000, -1.208970125616046080E-17, 6.505213034913038160E-19 ) ) ;
#12186 = CARTESIAN_POINT ( 'NONE',  ( -3.604218085003659588, 5.430620144867039478, 39.39148225573723749 ) ) ;
#12187 = VERTEX_POINT ( 'NONE', #10770 ) ;
#12188 = CARTESIAN_POINT ( 'NONE',  ( 34.84300730320200046, -6.953913411054821303, 3.000000000000056399 ) ) ;
#12189 = CARTESIAN_POINT ( 'NONE',  ( 5.422702462874749330, 33.99260377204210926, 40.31673423471877271 ) ) ;
#12190 = VERTEX_POINT ( 'NONE', #10653 ) ;
#12191 = CARTESIAN_POINT ( 'NONE',  ( 2.576224933359552605, 39.84426458497861034, -51.65025110506227435 ) ) ;
#12192 = CARTESIAN_POINT ( 'NONE',  ( -0.7806882667109514840, 39.98538465716378454, 49.65403242876611500 ) ) ;
#12193 = CYLINDRICAL_SURFACE ( 'NONE', #21572, 1.000000000000000888 ) ;
#12194 = AXIS2_PLACEMENT_3D ( 'NONE', #21716, #5554, #19546 ) ;
#12195 = CARTESIAN_POINT ( 'NONE',  ( 35.33352588067123179, 7.094908322882953478, 3.000000000000009770 ) ) ;
#12196 = DIRECTION ( 'NONE',  ( -0.000000000000000000, 1.000000000000000000, -0.000000000000000000 ) ) ;
#12197 = AXIS2_PLACEMENT_3D ( 'NONE', #21408, #5377, #19470 ) ;
#12198 = CIRCLE ( 'NONE', #16214, 1.000000000000000888 ) ;
#12199 = DIRECTION ( 'NONE',  ( 1.296372316667914327E-16, 1.000000000000000000, -0.000000000000000000 ) ) ;
#12201 = ORIENTED_EDGE ( 'NONE', *, *, #21092, .F. ) ;
#12200 = EDGE_CURVE ( 'NONE', #20409, #2631, #2083, .T. ) ;
#12202 = VERTEX_POINT ( 'NONE', #9075 ) ;
#12203 = ORIENTED_EDGE ( 'NONE', *, *, #1377, .F. ) ;
#12204 = ORIENTED_EDGE ( 'NONE', *, *, #11747, .T. ) ;
#12205 = DIRECTION ( 'NONE',  ( 6.505213034913038160E-19, 3.903127820947822896E-18, 1.000000000000000000 ) ) ;
#12206 = EDGE_CURVE ( 'NONE', #6302, #13976, #8180, .T. ) ;
#12207 = CARTESIAN_POINT ( 'NONE',  ( 42.50000000000000711, -5.000000000000000000, 49.60000000000000853 ) ) ;
#12208 = B_SPLINE_SURFACE_WITH_KNOTS ( 'NONE', 1, 3, ( 
 ( #21813, #20093, #4398, #2910, #11373, #2789, #20321, #11714, #20886, #9983, #15248, #21, #20646, #13968, #7011, #1285, #20766, #17202, #4745, #3015 ),
 ( #22268, #10315, #15705, #8277, #17311, #5078, #17089, #1515, #12055, #8498, #16976, #15472, #3243, #22612, #5186, #22492, #18710, #6566, #13527, #3122 ) ),
 .UNSPECIFIED., .F., .F., .F.,
 ( 2, 2 ),
 ( 4, 2, 2, 2, 2, 2, 2, 2, 2, 4 ),
 ( 0.000000000000000000, 1.000000000000000000 ),
 ( 0.000000000000000000, 0.002777081730120475617, 0.004165622595180713643, 0.005554163460240951235, 0.006942704325301189694, 0.008331245190361427286, 0.009025515622891545214, 0.009719786055421664878, 0.01041405648795178454, 0.01110832692048190247 ),
 .UNSPECIFIED. ) ;
#12209 = AXIS2_PLACEMENT_3D ( 'NONE', #11282, #3035, #20340 ) ;
#12210 = AXIS2_PLACEMENT_3D ( 'NONE', #4716, #4598, #20177 ) ;
#12211 = CARTESIAN_POINT ( 'NONE',  ( 3.266360431321861887E-15, -2.999999999999995559, 0.000000000000000000 ) ) ;
#12212 = CARTESIAN_POINT ( 'NONE',  ( 8.646032897229233072, -31.21605069118116305, 2.999999999999995559 ) ) ;
#12213 = CARTESIAN_POINT ( 'NONE',  ( 0.06362111936223997788, 39.99997618853521431, 48.78343666895094088 ) ) ;
#12214 = EDGE_LOOP ( 'NONE', ( #19722, #11620, #628, #2320 ) ) ;
#12215 = CARTESIAN_POINT ( 'NONE',  ( -42.50000000000000711, -12.00000000000012434, 47.50000000000000711 ) ) ;
#12216 = DIRECTION ( 'NONE',  ( 6.505213034913038160E-19, 3.903127820947822896E-18, 1.000000000000000000 ) ) ;
#12217 = DIRECTION ( 'NONE',  ( 1.000000000000000000, -1.084202172485505420E-16, 0.000000000000000000 ) ) ;
#12218 = DIRECTION ( 'NONE',  ( 0.000000000000000000, 0.000000000000000000, -1.000000000000000000 ) ) ;
#12219 = AXIS2_PLACEMENT_3D ( 'NONE', #11041, #2345, #16433 ) ;
#12220 = EDGE_CURVE ( 'NONE', #16743, #1869, #14004, .T. ) ;
#12221 = VERTEX_POINT ( 'NONE', #5626 ) ;
#12222 = AXIS2_PLACEMENT_3D ( 'NONE', #18891, #6290, #2975 ) ;
#12223 = LINE ( 'NONE', #7302, #21369 ) ;
#12224 = CYLINDRICAL_SURFACE ( 'NONE', #4581, 18.00000000000000000 ) ;
#12225 = FACE_BOUND ( 'NONE', #4138, .T. ) ;
#12226 = EDGE_CURVE ( 'NONE', #13393, #15368, #20600, .T. ) ;
#12227 = EDGE_LOOP ( 'NONE', ( #16247, #18666, #18203, #20393 ) ) ;
#12228 = VERTEX_POINT ( 'NONE', #12831 ) ;
#12229 = EDGE_LOOP ( 'NONE', ( #12765, #18093 ) ) ;
#12230 = APPLICATION_CONTEXT ( 'automotive_design' ) ;
#12231 = CARTESIAN_POINT ( 'NONE',  ( 0.6683989176551251576, -3.155640224521520043, -47.80307817979551288 ) ) ;
#12232 = CARTESIAN_POINT ( 'NONE',  ( 1.102182119232617517E-15, 30.00000000000000000, 8.999999999999998224 ) ) ;
#12233 = VERTEX_POINT ( 'NONE', #18002 ) ;
#12234 = FACE_OUTER_BOUND ( 'NONE', #842, .T. ) ;
#12235 = B_SPLINE_CURVE_WITH_KNOTS ( 'NONE', 3,
 ( #3769, #322, #10970, #2265, #5703, #7655, #12452, #1928, #21066, #9028, #12564, #9249, #7312, #14277, #21294, #5583, #16234, #19575, #3883, #10850 ),
 .UNSPECIFIED., .F., .F.,
 ( 4, 2, 2, 2, 2, 2, 2, 2, 2, 4 ),
 ( 0.02328883130680912961, 0.02567687977621935583, 0.02687090401092446373, 0.02806492824562957511, 0.03284102518444999286, 0.03522907365386020867, 0.03761712212327042448, 0.03881114635797552198, 0.04000517059268062642, 0.04239321906209084223 ),
 .UNSPECIFIED. ) ;
#12236 = CARTESIAN_POINT ( 'NONE',  ( 5.833333333333328596, 33.81926995981416439, -40.61164310337066041 ) ) ;
#12237 = DIRECTION ( 'NONE',  ( 0.000000000000000000, 1.000000000000000000, 0.000000000000000000 ) ) ;
#12238 = CARTESIAN_POINT ( 'NONE',  ( -18.68837533793345784, 7.522086334128091245, -57.74247137455871126 ) ) ;
#12239 = AXIS2_PLACEMENT_3D ( 'NONE', #1998, #9207, #10923 ) ;
#12240 = LINE ( 'NONE', #19245, #8980 ) ;
#12241 = EDGE_CURVE ( 'NONE', #16483, #10675, #11831, .T. ) ;
#12242 = EDGE_LOOP ( 'NONE', ( #10693, #11484, #10112, #6627 ) ) ;
#12243 = CARTESIAN_POINT ( 'NONE',  ( 6.000000000000000888, -40.00000000000000000, 6.000000000000000000 ) ) ;
#12244 = LINE ( 'NONE', #19251, #18897 ) ;
#12245 = CARTESIAN_POINT ( 'NONE',  ( 11.38359864655681086, 10.20536502146449109, -44.07478837098130242 ) ) ;
#12246 = ORIENTED_EDGE ( 'NONE', *, *, #15530, .F. ) ;
#12247 = CARTESIAN_POINT ( 'NONE',  ( -35.00000000000000000, -9.000000000000001776, 1.387778780781445676E-14 ) ) ;
#12248 = CARTESIAN_POINT ( 'NONE',  ( 25.58633464742662866, 23.74488952252781715, 2.999999999999999112 ) ) ;
#12249 = EDGE_CURVE ( 'NONE', #6323, #6579, #117, .T. ) ;
#12250 = EDGE_CURVE ( 'NONE', #12705, #19146, #8903, .T. ) ;
#12251 = EDGE_CURVE ( 'NONE', #15720, #15515, #7694, .T. ) ;
#12252 = AXIS2_PLACEMENT_3D ( 'NONE', #12913, #14858, #19713 ) ;
#12253 = ORIENTED_EDGE ( 'NONE', *, *, #3080, .T. ) ;
#12254 = EDGE_CURVE ( 'NONE', #3930, #22344, #15845, .T. ) ;
#12255 = AXIS2_PLACEMENT_3D ( 'NONE', #18718, #9894, #16883 ) ;
#12256 = ORIENTED_EDGE ( 'NONE', *, *, #6377, .T. ) ;
#12257 = CARTESIAN_POINT ( 'NONE',  ( 2.999999999999999556, 22.00000000000000000, 8.485281374238567764 ) ) ;
#12258 = LINE ( 'NONE', #107, #20185 ) ;
#12259 = AXIS2_PLACEMENT_3D ( 'NONE', #22459, #15214, #13717 ) ;
#12260 = FACE_OUTER_BOUND ( 'NONE', #4665, .T. ) ;
#12261 = CARTESIAN_POINT ( 'NONE',  ( 2.602085213965210642E-15, -0.9047447100419790944, 0.000000000000000000 ) ) ;
#12262 = CARTESIAN_POINT ( 'NONE',  ( 5.093313992686421265, 32.09841355225992743, 3.000000000000023537 ) ) ;
#12263 = VERTEX_POINT ( 'NONE', #12943 ) ;
#12264 = LINE ( 'NONE', #18813, #2522 ) ;
#12265 = CARTESIAN_POINT ( 'NONE',  ( 25.99999999999998579, 19.99999999999999645, 105.0000000000000142 ) ) ;
#12266 = ORIENTED_EDGE ( 'NONE', *, *, #1382, .T. ) ;
#12267 = CARTESIAN_POINT ( 'NONE',  ( 0.000000000000000000, 15.00000000000000355, 0.000000000000000000 ) ) ;
#12268 = CARTESIAN_POINT ( 'NONE',  ( 0.000000000000000000, -1.500000000000015099, 0.000000000000000000 ) ) ;
#12269 = VECTOR ( 'NONE', #10644, 999.9999999999998863 ) ;
#12270 = CARTESIAN_POINT ( 'NONE',  ( -35.00000000000000000, 25.00000000000000000, 17.00000000000002487 ) ) ;
#12271 = CYLINDRICAL_SURFACE ( 'NONE', #11964, 19.11328065563152023 ) ;
#12272 = CARTESIAN_POINT ( 'NONE',  ( 6.426802710256903417, 33.56875711009141838, -41.03786381671498873 ) ) ;
#12273 = VERTEX_POINT ( 'NONE', #6088 ) ;
#12274 = CARTESIAN_POINT ( 'NONE',  ( -26.50842683089750551, 24.41514043009185286, 2.999999999999995559 ) ) ;
#12275 = CARTESIAN_POINT ( 'NONE',  ( -21.20802570598058878, 27.37171784732027291, 58.39394879075536693 ) ) ;
#12276 = ORIENTED_EDGE ( 'NONE', *, *, #9164, .F. ) ;
#12277 = CARTESIAN_POINT ( 'NONE',  ( -5.833333333333329485, 0.000000000000000000, 40.61164310337067462 ) ) ;
#12278 = DIRECTION ( 'NONE',  ( 0.000000000000000000, 0.000000000000000000, 1.000000000000000000 ) ) ;
#12279 = DIRECTION ( 'NONE',  ( -1.000000000000000000, 1.020425574104004122E-16, 0.000000000000000000 ) ) ;
#12280 = AXIS2_PLACEMENT_3D ( 'NONE', #19615, #7464, #21109 ) ;
#12281 = AXIS2_PLACEMENT_3D ( 'NONE', #10598, #67, #21044 ) ;
#12282 = AXIS2_PLACEMENT_3D ( 'NONE', #12435, #3750, #10709 ) ;
#12283 = B_SPLINE_CURVE_WITH_KNOTS ( 'NONE', 3,
 ( #14023, #12433, #3748, #21270 ),
 .UNSPECIFIED., .F., .F.,
 ( 4, 4 ),
 ( 9.545285770168743104E-07, 0.001900595205834662181 ),
 .UNSPECIFIED. ) ;
#12284 = CIRCLE ( 'NONE', #5346, 2.499999999999998668 ) ;
#12286 = EDGE_CURVE ( 'NONE', #14574, #16276, #2691, .T. ) ;
#12285 = ORIENTED_EDGE ( 'NONE', *, *, #18744, .F. ) ;
#12287 = CIRCLE ( 'NONE', #9369, 60.00000000000000000 ) ;
#12288 = EDGE_CURVE ( 'NONE', #5141, #12838, #2616, .T. ) ;
#12289 = ORIENTED_EDGE ( 'NONE', *, *, #4592, .F. ) ;
#12290 = ORIENTED_EDGE ( 'NONE', *, *, #15184, .F. ) ;
#12291 = ORIENTED_EDGE ( 'NONE', *, *, #7090, .F. ) ;
#12292 = CARTESIAN_POINT ( 'NONE',  ( -2.615700731179644301, 23.51654087860100262, 6.612978332543312021 ) ) ;
#12293 = CYLINDRICAL_SURFACE ( 'NONE', #4890, 49.99999999999998579 ) ;
#12294 = DIRECTION ( 'NONE',  ( 6.505213034913038160E-19, 3.903127820947822896E-18, 1.000000000000000000 ) ) ;
#12295 = EDGE_CURVE ( 'NONE', #1418, #7291, #16953, .T. ) ;
#12296 = VERTEX_POINT ( 'NONE', #13391 ) ;
#12297 = CARTESIAN_POINT ( 'NONE',  ( -34.99999999999999289, -1.000000000000028644, -3.012171160963566127E-14 ) ) ;
#12298 = CARTESIAN_POINT ( 'NONE',  ( -2.605854907981514312, 5.225826804957995009, 39.07589943342649974 ) ) ;
#12299 = VERTEX_POINT ( 'NONE', #18455 ) ;
#12300 = CIRCLE ( 'NONE', #11939, 0.9999999999999974465 ) ;
#12301 = VECTOR ( 'NONE', #12563, 1000.000000000000000 ) ;
#12302 = VECTOR ( 'NONE', #17093, 1000.000000000000000 ) ;
#12303 = CARTESIAN_POINT ( 'NONE',  ( 2.220446049250313081E-13, -2.498001805406602216E-13, -6.859353255829918616 ) ) ;
#12304 = AXIS2_PLACEMENT_3D ( 'NONE', #11904, #18909, #10181 ) ;
#12305 = CARTESIAN_POINT ( 'NONE',  ( 34.24928931925769149, -6.742883674876604339, 3.000000000000002665 ) ) ;
#12306 = ORIENTED_EDGE ( 'NONE', *, *, #20161, .F. ) ;
#12307 = CARTESIAN_POINT ( 'NONE',  ( 5.833333333333338366, 33.81926995981415729, 40.61164310337067462 ) ) ;
#12308 = CARTESIAN_POINT ( 'NONE',  ( -8.331955809010628045, 38.18181818181818699, 56.36098470834075158 ) ) ;
#12309 = CARTESIAN_POINT ( 'NONE',  ( 35.00000000000058265, 39.97500000000000142, -57.50000000000076028 ) ) ;
#12310 = CARTESIAN_POINT ( 'NONE',  ( 17.35828117057767273, 30.07901706855390600, 57.39628071424991873 ) ) ;
#12311 = CARTESIAN_POINT ( 'NONE',  ( -25.00000000000000000, -20.00000000000000000, -25.00000000000000000 ) ) ;
#12312 = DIRECTION ( 'NONE',  ( 0.000000000000000000, 1.000000000000000000, 0.000000000000000000 ) ) ;
#12313 = AXIS2_PLACEMENT_3D ( 'NONE', #923, #4256, #14428 ) ;
#12314 = ORIENTED_EDGE ( 'NONE', *, *, #11273, .F. ) ;
#12315 = ORIENTED_EDGE ( 'NONE', *, *, #8390, .F. ) ;
#12316 = ORIENTED_EDGE ( 'NONE', *, *, #18899, .F. ) ;
#12317 = ORIENTED_EDGE ( 'NONE', *, *, #18317, .F. ) ;
#12318 = CARTESIAN_POINT ( 'NONE',  ( 2.775557561562891351E-14, -2.775557561562891351E-14, 2.999999999999999112 ) ) ;
#12319 = AXIS2_PLACEMENT_3D ( 'NONE', #5432, #7598, #17678 ) ;
#12320 = DIRECTION ( 'NONE',  ( 1.000000000000000000, 1.208970125616063798E-17, 0.000000000000000000 ) ) ;
#12321 = CARTESIAN_POINT ( 'NONE',  ( 2.422192751863949667, 32.40961249803550714, 2.999999999999995559 ) ) ;
#12322 = CARTESIAN_POINT ( 'NONE',  ( 1.038202552616665164, 39.99359457986729893, 49.52478249909115959 ) ) ;
#12323 = ORIENTED_EDGE ( 'NONE', *, *, #443, .F. ) ;
#12324 = CARTESIAN_POINT ( 'NONE',  ( -4.171001175319349663, -35.79662727779881237, -6.999999999999964473 ) ) ;
#12325 = CIRCLE ( 'NONE', #2465, 60.00000000000000000 ) ;
#12326 = DIRECTION ( 'NONE',  ( 0.000000000000000000, 0.000000000000000000, 1.000000000000000000 ) ) ;
#12327 = DIRECTION ( 'NONE',  ( 6.505213034913038160E-19, 3.903127820947822896E-18, 1.000000000000000000 ) ) ;
#12328 = DIRECTION ( 'NONE',  ( -0.000000000000000000, -1.000000000000000000, -0.000000000000000000 ) ) ;
#12329 = CIRCLE ( 'NONE', #12341, 15.00000000000000000 ) ;
#12330 = EDGE_CURVE ( 'NONE', #15787, #9204, #816, .T. ) ;
#12331 = CARTESIAN_POINT ( 'NONE',  ( -19.41351212956693573, 24.83257706694780609, 60.47995209899217883 ) ) ;
#12332 = CARTESIAN_POINT ( 'NONE',  ( 35.00000000000000000, 15.00000000000000000, -40.99999999999997868 ) ) ;
#12333 = EDGE_CURVE ( 'NONE', #10809, #1823, #11856, .T. ) ;
#12334 = CARTESIAN_POINT ( 'NONE',  ( -7.073836202554792507, 38.72384538518738140, 54.13588025449750063 ) ) ;
#12335 = DIRECTION ( 'NONE',  ( -0.000000000000000000, 1.000000000000000000, -0.000000000000000000 ) ) ;
#12336 = CARTESIAN_POINT ( 'NONE',  ( 90.00000000000000000, 26.00000000000000355, -9.108981535246192915E-16 ) ) ;
#12337 = B_SPLINE_CURVE_WITH_KNOTS ( 'NONE', 3,
 ( #15612, #374, #22637, #3714, #8856, #139, #1770, #6929, #15827, #5207, #7365, #21123, #13889, #17670, #7135, #20905, #1981, #17337, #5424, #14102, #1654, #21341, #5526, #19629, #10664, #16065, #12402, #14333, #3937, #1874, #5639, #256, #7252, #8633, #17449, #12183, #8964, #8755, #19185, #13985, #3491, #10450, #19413, #15725, #38, #15944, #10785, #7028, #3820 ),
 .UNSPECIFIED., .F., .F.,
 ( 4, 1, 1, 1, 2, 2, 1, 1, 1, 1, 2, 2, 1, 1, 1, 2, 2, 1, 1, 1, 1, 2, 2, 1, 1, 1, 1, 2, 2, 1, 1, 1, 2, 2, 4 ),
 ( 0.000000000000000000, 0.1249999999999921729, 0.1874999999999877598, 0.2187499999999850953, 0.2343749999999842626, 0.2499999999999834577, 0.3749999999999780731, 0.4374999999999754086, 0.4687499999999746314, 0.4843749999999746314, 0.4921874999999742428, 0.4999999999999739098, 0.5624999999999701350, 0.5937499999999682476, 0.6093749999999673594, 0.6171874999999674705, 0.6249999999999674705, 0.6874999999999683586, 0.7187499999999685807, 0.7343749999999686917, 0.7421874999999690248, 0.7460937499999691358, 0.7499999999999692468, 0.8124999999999739098, 0.8437499999999762412, 0.8593749999999771294, 0.8671874999999773515, 0.8710937499999776845, 0.8749999999999779066, 0.9062499999999816813, 0.9218749999999836797, 0.9296874999999847899, 0.9335937499999855671, 0.9374999999999864553, 1.000000000000000000 ),
 .UNSPECIFIED. ) ;
#12338 = ORIENTED_EDGE ( 'NONE', *, *, #16022, .T. ) ;
#12339 = ORIENTED_EDGE ( 'NONE', *, *, #13548, .T. ) ;
#12340 = AXIS2_PLACEMENT_3D ( 'NONE', #6903, #1741, #18930 ) ;
#12341 = AXIS2_PLACEMENT_3D ( 'NONE', #17626, #1932, #15892 ) ;
#12342 = VERTEX_POINT ( 'NONE', #20072 ) ;
#12343 = CARTESIAN_POINT ( 'NONE',  ( -7.197698565811593951, -35.43359966464136335, 2.932460736555830394 ) ) ;
#12344 = CARTESIAN_POINT ( 'NONE',  ( -35.00000000000000000, 25.00000000000000000, 1.387778780781445676E-14 ) ) ;
#12345 = VECTOR ( 'NONE', #4752, 1000.000000000000000 ) ;
#12346 = AXIS2_PLACEMENT_3D ( 'NONE', #1056, #2777, #19964 ) ;
#12347 = DIRECTION ( 'NONE',  ( -0.000000000000000000, -1.000000000000000000, -0.000000000000000000 ) ) ;
#12348 = FACE_OUTER_BOUND ( 'NONE', #11120, .T. ) ;
#12349 = EDGE_CURVE ( 'NONE', #19349, #12202, #20182, .T. ) ;
#12350 = CARTESIAN_POINT ( 'NONE',  ( -14.19004819996300348, 37.38003124960519585, -56.27686160268856952 ) ) ;
#12351 = FACE_OUTER_BOUND ( 'NONE', #9742, .T. ) ;
#12352 = CIRCLE ( 'NONE', #9076, 18.00000000000000000 ) ;
#12353 = EDGE_LOOP ( 'NONE', ( #20495, #14662, #11759, #13647 ) ) ;
#12354 = DIRECTION ( 'NONE',  ( 1.000000000000000000, -1.296372316667914327E-16, 0.000000000000000000 ) ) ;
#12355 = AXIS2_PLACEMENT_3D ( 'NONE', #8670, #9931, #4899 ) ;
#12356 = FACE_BOUND ( 'NONE', #4808, .T. ) ;
#12357 = CARTESIAN_POINT ( 'NONE',  ( 24.73600648735124707, -27.19760187735892387, -2.800654218530457484 ) ) ;
#12358 = CARTESIAN_POINT ( 'NONE',  ( 11.84669267190943209, 10.76938159504123149, -44.31876460048058419 ) ) ;
#12359 = EDGE_CURVE ( 'NONE', #13092, #16803, #6368, .T. ) ;
#12360 = ORIENTED_EDGE ( 'NONE', *, *, #4345, .F. ) ;
#12361 = CARTESIAN_POINT ( 'NONE',  ( 4.080045426412798548, -32.20238537491815123, -6.999999999999950262 ) ) ;
#12362 = DIRECTION ( 'NONE',  ( 0.000000000000000000, -1.000000000000000000, 0.000000000000000000 ) ) ;
#12363 = AXIS2_PLACEMENT_3D ( 'NONE', #22014, #4147, #11232 ) ;
#12364 = ORIENTED_EDGE ( 'NONE', *, *, #19206, .F. ) ;
#12365 = AXIS2_PLACEMENT_3D ( 'NONE', #6354, #6471, #2590 ) ;
#12366 = VECTOR ( 'NONE', #10918, 1000.000000000000000 ) ;
#12367 = EDGE_CURVE ( 'NONE', #2168, #11124, #10781, .T. ) ;
#12368 = VECTOR ( 'NONE', #9912, 1000.000000000000000 ) ;
#12369 = AXIS2_PLACEMENT_3D ( 'NONE', #12844, #22670, #15641 ) ;
#12370 = VERTEX_POINT ( 'NONE', #15000 ) ;
#12371 = DIRECTION ( 'NONE',  ( 0.000000000000000000, 0.000000000000000000, -1.000000000000000000 ) ) ;
#12372 = DIRECTION ( 'NONE',  ( -0.000000000000000000, 1.000000000000000000, -0.000000000000000000 ) ) ;
#12373 = CARTESIAN_POINT ( 'NONE',  ( 12.00937115242667375, 34.74700806321082069, -2.800654218530485018 ) ) ;
#12374 = ORIENTED_EDGE ( 'NONE', *, *, #17048, .T. ) ;
#12375 = DIRECTION ( 'NONE',  ( 0.000000000000000000, -1.000000000000000000, 0.000000000000000000 ) ) ;
#12376 = CARTESIAN_POINT ( 'NONE',  ( -10.34137811700765397, 39.99999999999997868, 53.75702834151201870 ) ) ;
#12377 = ORIENTED_EDGE ( 'NONE', *, *, #9333, .T. ) ;
#12378 = EDGE_CURVE ( 'NONE', #8183, #12492, #22106, .T. ) ;
#12380 = EDGE_CURVE ( 'NONE', #6233, #18161, #4181, .T. ) ;
#12379 = DIRECTION ( 'NONE',  ( 0.000000000000000000, 0.000000000000000000, -1.000000000000000000 ) ) ;
#12381 = DIRECTION ( 'NONE',  ( -6.505213034913038160E-19, -3.903127820947822896E-18, -1.000000000000000000 ) ) ;
#12382 = DIRECTION ( 'NONE',  ( 1.224646799147353207E-16, 1.000000000000000000, -0.000000000000000000 ) ) ;
#12383 = CARTESIAN_POINT ( 'NONE',  ( -3.801357191711898231, 39.91216781306113859, -51.45795414075008267 ) ) ;
#12384 = ORIENTED_EDGE ( 'NONE', *, *, #7133, .F. ) ;
#12385 = DIRECTION ( 'NONE',  ( 6.505213034913038160E-19, 3.903127820947822896E-18, 1.000000000000000000 ) ) ;
#12386 = CARTESIAN_POINT ( 'NONE',  ( -15.12081897056651059, 33.51030287062345536, 2.800654218530485018 ) ) ;
#12387 = CARTESIAN_POINT ( 'NONE',  ( -5.042540965661301833, 39.84191928929035242, -52.23966299716700235 ) ) ;
#12388 = ORIENTED_EDGE ( 'NONE', *, *, #10126, .T. ) ;
#12389 = CARTESIAN_POINT ( 'NONE',  ( -1.387778780781445518E-14, 20.00000000000000355, -105.0000000000000142 ) ) ;
#12390 = CARTESIAN_POINT ( 'NONE',  ( -35.00000000000058265, 40.00000000000000711, -55.00000000000076028 ) ) ;
#12391 = ADVANCED_FACE ( 'NONE', ( #13167 ), #17691, .T. ) ;
#12392 = CARTESIAN_POINT ( 'NONE',  ( 0.6841746959068695233, 36.75746821813305587, 2.800654218530485018 ) ) ;
#12393 = CIRCLE ( 'NONE', #17516, 4.999999999999997335 ) ;
#12394 = ORIENTED_EDGE ( 'NONE', *, *, #19548, .T. ) ;
#12395 = ORIENTED_EDGE ( 'NONE', *, *, #1020, .T. ) ;
#12396 = ADVANCED_FACE ( 'NONE', ( #6310 ), #867, .T. ) ;
#12397 = ORIENTED_EDGE ( 'NONE', *, *, #14634, .F. ) ;
#12398 = ORIENTED_EDGE ( 'NONE', *, *, #540, .T. ) ;
#12399 = CARTESIAN_POINT ( 'NONE',  ( 9.952189117650862116, 40.00000000000000000, -53.64426396172072486 ) ) ;
#12400 = CARTESIAN_POINT ( 'NONE',  ( 12.60179598819646429, 38.53795549125497644, 55.66391160832503715 ) ) ;
#12401 = CARTESIAN_POINT ( 'NONE',  ( 0.7796804372245736969, 40.00000000000002132, -49.24007646455138598 ) ) ;
#12402 = CARTESIAN_POINT ( 'NONE',  ( 7.158017760915646122, 39.99999999999999289, 52.61520709092953041 ) ) ;
#12403 = VERTEX_POINT ( 'NONE', #18572 ) ;
#12404 = DIRECTION ( 'NONE',  ( -6.505213034913038160E-19, -3.903127820947822896E-18, -1.000000000000000000 ) ) ;
#12405 = CARTESIAN_POINT ( 'NONE',  ( -41.39271818392631985, 10.00000000000000000, 5.943569790512528428 ) ) ;
#12406 = ORIENTED_EDGE ( 'NONE', *, *, #11911, .F. ) ;
#12407 =( GEOMETRIC_REPRESENTATION_CONTEXT ( 3 ) GLOBAL_UNCERTAINTY_ASSIGNED_CONTEXT ( ( #20214 ) ) GLOBAL_UNIT_ASSIGNED_CONTEXT ( ( #17560, #16060, #14564 ) ) REPRESENTATION_CONTEXT ( 'NONE', 'WORKASPACE' ) );
#12408 = EDGE_CURVE ( 'NONE', #20709, #6187, #19174, .T. ) ;
#12409 = CARTESIAN_POINT ( 'NONE',  ( -18.32709649528716866, 33.00101640267667591, -57.63983358650814637 ) ) ;
#12410 = DIRECTION ( 'NONE',  ( 0.000000000000000000, 0.000000000000000000, -1.000000000000000000 ) ) ;
#12411 = CARTESIAN_POINT ( 'NONE',  ( 7.545596340795487578, -0.4932457138281565179, 52.99914579202447129 ) ) ;
#12412 = VERTEX_POINT ( 'NONE', #2886 ) ;
#12413 = CARTESIAN_POINT ( 'NONE',  ( -35.00000000000058265, 39.97500000000000142, -52.50000000000076739 ) ) ;
#12414 = EDGE_CURVE ( 'NONE', #11550, #10912, #16855, .T. ) ;
#12415 = CARTESIAN_POINT ( 'NONE',  ( -90.00000000000000000, 39.97500000000000142, -2.500000000000003109 ) ) ;
#12416 = CIRCLE ( 'NONE', #14235, 6.499999999999999112 ) ;
#12417 = CARTESIAN_POINT ( 'NONE',  ( 17.76477806472427545, 33.73774409952945064, 57.47211831788253278 ) ) ;
#12418 = LINE ( 'NONE', #5221, #13610 ) ;
#12419 = DIRECTION ( 'NONE',  ( -1.000000000000000000, 1.301042606982605814E-16, 0.000000000000000000 ) ) ;
#12420 = VERTEX_POINT ( 'NONE', #22129 ) ;
#12421 = ORIENTED_EDGE ( 'NONE', *, *, #3728, .F. ) ;
#12422 = ORIENTED_EDGE ( 'NONE', *, *, #5104, .T. ) ;
#12423 = ORIENTED_EDGE ( 'NONE', *, *, #4016, .F. ) ;
#12424 = DIRECTION ( 'NONE',  ( -0.000000000000000000, -1.000000000000000000, -0.000000000000000000 ) ) ;
#12425 = PLANE ( 'NONE',  #1580 ) ;
#12426 = DIRECTION ( 'NONE',  ( -0.5002637533272169534, 0.000000000000000000, -0.8658730721687594167 ) ) ;
#12427 = AXIS2_PLACEMENT_3D ( 'NONE', #3069, #20712, #8337 ) ;
#12428 = CARTESIAN_POINT ( 'NONE',  ( -34.65667543218827973, -4.170748987303380062, 3.000000000000002665 ) ) ;
#12429 = CARTESIAN_POINT ( 'NONE',  ( 35.00000000000000000, 10.00000000000000000, 2.365113165210053967E-14 ) ) ;
#12430 = CARTESIAN_POINT ( 'NONE',  ( 0.2542260610985473956, 39.99961928011452983, 48.93085117298642928 ) ) ;
#12431 = ORIENTED_EDGE ( 'NONE', *, *, #12220, .T. ) ;
#12432 = CYLINDRICAL_SURFACE ( 'NONE', #10186, 2.500000000000002220 ) ;
#12433 = CARTESIAN_POINT ( 'NONE',  ( 32.89319786336257323, 15.00354810072174239, -2.933296326616365857 ) ) ;
#12434 = CARTESIAN_POINT ( 'NONE',  ( 42.50000000000000711, -12.00000000000000000, -41.00000000000000000 ) ) ;
#12435 = CARTESIAN_POINT ( 'NONE',  ( -35.00000000000000000, -9.000000000000001776, 1.387778780781445676E-14 ) ) ;
#12436 =( NAMED_UNIT ( * ) SI_UNIT ( $, .STERADIAN. ) SOLID_ANGLE_UNIT ( ) );
#12437 = ADVANCED_FACE ( 'NONE', ( #18689 ), #14765, .F. ) ;
#12438 = AXIS2_PLACEMENT_3D ( 'NONE', #21311, #7560, #14538 ) ;
#12439 = DIRECTION ( 'NONE',  ( 0.000000000000000000, 0.000000000000000000, -1.000000000000000000 ) ) ;
#12440 = CARTESIAN_POINT ( 'NONE',  ( 3.460816278822046447E-15, -1.500000000000011768, 0.000000000000000000 ) ) ;
#12441 = EDGE_CURVE ( 'NONE', #14737, #586, #9528, .T. ) ;
#12442 = DIRECTION ( 'NONE',  ( 0.000000000000000000, -1.000000000000000000, 0.000000000000000000 ) ) ;
#12443 = ORIENTED_EDGE ( 'NONE', *, *, #13091, .F. ) ;
#12444 = ORIENTED_EDGE ( 'NONE', *, *, #15293, .T. ) ;
#12445 = B_SPLINE_CURVE_WITH_KNOTS ( 'NONE', 3,
 ( #20922, #17692, #14240, #12522 ),
 .UNSPECIFIED., .F., .F.,
 ( 4, 4 ),
 ( 9.715086411272982943E-07, 0.001929643240672562375 ),
 .UNSPECIFIED. ) ;
#12446 = ORIENTED_EDGE ( 'NONE', *, *, #4292, .T. ) ;
#12447 = CARTESIAN_POINT ( 'NONE',  ( 4.842578813366696266, -0.8535550256994554053, -51.47191290771694838 ) ) ;
#12448 = AXIS2_PLACEMENT_3D ( 'NONE', #2036, #12674, #19695 ) ;
#12449 = DIRECTION ( 'NONE',  ( 0.9659258262890679791, 0.2588190451025219052, 1.182917971378669349E-16 ) ) ;
#12450 = ADVANCED_FACE ( 'NONE', ( #18913 ), #20745, .F. ) ;
#12451 = DIRECTION ( 'NONE',  ( 6.505213034913038160E-19, 3.903127820947822896E-18, 1.000000000000000000 ) ) ;
#12452 = CARTESIAN_POINT ( 'NONE',  ( -19.52068517772380574, 15.62943592677016191, 60.50640500721819848 ) ) ;
#12453 = CARTESIAN_POINT ( 'NONE',  ( 30.99230043872329432, -17.38334492574589163, -2.999999999999984901 ) ) ;
#12454 = CARTESIAN_POINT ( 'NONE',  ( 22.28024240313511584, 22.26748298433259166, -2.999999999999999112 ) ) ;
#12455 = ORIENTED_EDGE ( 'NONE', *, *, #8147, .F. ) ;
#12456 = DIRECTION ( 'NONE',  ( 0.000000000000000000, 0.000000000000000000, 1.000000000000000000 ) ) ;
#12457 = CARTESIAN_POINT ( 'NONE',  ( -5.833333333333341919, 33.81926995981417150, -40.61164310337066041 ) ) ;
#12458 = CARTESIAN_POINT ( 'NONE',  ( -35.00000000000058265, 26.00000000000000355, -55.00000000000076028 ) ) ;
#12459 = CARTESIAN_POINT ( 'NONE',  ( 14.76055860720887836, 17.30233064284068334, -45.72055682016586076 ) ) ;
#12460 = ORIENTED_EDGE ( 'NONE', *, *, #19649, .F. ) ;
#12461 = AXIS2_PLACEMENT_3D ( 'NONE', #19965, #4276, #9761 ) ;
#12462 = CARTESIAN_POINT ( 'NONE',  ( 17.00000000000001421, 0.6398376396478597794, 2.081899558550501463E-15 ) ) ;
#12463 = B_SPLINE_CURVE_WITH_KNOTS ( 'NONE', 3,
 ( #448, #2177, #10993, #2286 ),
 .UNSPECIFIED., .F., .F.,
 ( 4, 4 ),
 ( 0.001875451646903029826, 0.003761979286331461510 ),
 .UNSPECIFIED. ) ;
#12464 = CARTESIAN_POINT ( 'NONE',  ( -20.06142356895407275, 29.33203831401573325, 3.000000000000061284 ) ) ;
#12465 = ORIENTED_EDGE ( 'NONE', *, *, #16184, .F. ) ;
#12466 = ADVANCED_FACE ( 'NONE', ( #12035 ), #13608, .T. ) ;
#12467 = CIRCLE ( 'NONE', #6632, 4.000000000000000000 ) ;
#12468 = ORIENTED_EDGE ( 'NONE', *, *, #1237, .F. ) ;
#12469 = CARTESIAN_POINT ( 'NONE',  ( -1.387778780781445676E-14, 40.00000000000000000, -48.73397172404481381 ) ) ;
#12470 = EDGE_CURVE ( 'NONE', #7599, #7962, #18474, .T. ) ;
#12471 = DIRECTION ( 'NONE',  ( -1.000000000000000000, -1.208970125616060717E-17, 0.000000000000000000 ) ) ;
#12472 = CARTESIAN_POINT ( 'NONE',  ( 90.00000000000000000, 28.00000000000000000, 2.500000000000001332 ) ) ;
#12473 = DIRECTION ( 'NONE',  ( -0.000000000000000000, 1.000000000000000000, -0.000000000000000000 ) ) ;
#12474 = VERTEX_POINT ( 'NONE', #1838 ) ;
#12475 = CARTESIAN_POINT ( 'NONE',  ( 42.50000000000000711, -11.97499999999999964, -47.50000000000000000 ) ) ;
#12476 = CARTESIAN_POINT ( 'NONE',  ( -8.835430549262724753, 40.00000000000000711, 53.27933386073573985 ) ) ;
#12477 = ORIENTED_EDGE ( 'NONE', *, *, #20243, .F. ) ;
#12478 = CARTESIAN_POINT ( 'NONE',  ( 25.99999999999998579, 19.99999999999999645, -105.0010000000000048 ) ) ;
#12479 = CARTESIAN_POINT ( 'NONE',  ( 16.84758200736122546, 5.154512310752989102, -57.18908790048117652 ) ) ;
#12480 = DIRECTION ( 'NONE',  ( 6.505213034913038160E-19, 3.903127820947822896E-18, 1.000000000000000000 ) ) ;
#12481 = EDGE_LOOP ( 'NONE', ( #16641, #15937, #19423, #21834 ) ) ;
#12482 = FACE_OUTER_BOUND ( 'NONE', #22254, .T. ) ;
#12483 = DIRECTION ( 'NONE',  ( 0.000000000000000000, 1.000000000000000000, 0.000000000000000000 ) ) ;
#12484 = CARTESIAN_POINT ( 'NONE',  ( -6.646840153610217961, 39.71385754597948647, -53.15684335981527653 ) ) ;
#12485 = ORIENTED_EDGE ( 'NONE', *, *, #6467, .T. ) ;
#12486 = CONICAL_SURFACE ( 'NONE', #8842, 9.000000000000035527, 0.7853981633974447263 ) ;
#12487 = EDGE_CURVE ( 'NONE', #12153, #2477, #18804, .T. ) ;
#12488 = DIRECTION ( 'NONE',  ( 0.000000000000000000, 0.000000000000000000, -1.000000000000000000 ) ) ;
#12489 = CARTESIAN_POINT ( 'NONE',  ( 3.608224830031758756E-13, -2.775557561562891351E-14, -4.999999999999997335 ) ) ;
#12490 = EDGE_CURVE ( 'NONE', #20847, #5303, #20620, .T. ) ;
#12491 = EDGE_CURVE ( 'NONE', #15447, #16688, #21363, .T. ) ;
#12492 = VERTEX_POINT ( 'NONE', #3341 ) ;
#12493 = VERTEX_POINT ( 'NONE', #1379 ) ;
#12494 = ORIENTED_EDGE ( 'NONE', *, *, #17408, .F. ) ;
#12495 =( NAMED_UNIT ( * ) PLANE_ANGLE_UNIT ( ) SI_UNIT ( $, .RADIAN. ) );
#12496 = ORIENTED_EDGE ( 'NONE', *, *, #5369, .T. ) ;
#12497 = CARTESIAN_POINT ( 'NONE',  ( 34.00000000000000000, 8.251288694035739724, 4.163799117100999770E-15 ) ) ;
#12498 = CARTESIAN_POINT ( 'NONE',  ( -25.58633464742629471, -23.74488952252781715, -2.999999999999975131 ) ) ;
#12499 = AXIS2_PLACEMENT_3D ( 'NONE', #13382, #11784, #11900 ) ;
#12500 = CARTESIAN_POINT ( 'NONE',  ( 2.636011669654858558, 39.95887917521793753, -50.67499985581887501 ) ) ;
#12501 = DIRECTION ( 'NONE',  ( -1.000000000000000000, 0.000000000000000000, 0.000000000000000000 ) ) ;
#12502 = ORIENTED_EDGE ( 'NONE', *, *, #12665, .T. ) ;
#12503 = DIRECTION ( 'NONE',  ( -0.000000000000000000, -0.000000000000000000, -1.000000000000000000 ) ) ;
#12504 = CARTESIAN_POINT ( 'NONE',  ( -31.47226199422867410, 17.79229176513279498, -2.933296326616379623 ) ) ;
#12505 = EDGE_LOOP ( 'NONE', ( #1655, #8126, #21738, #14212 ) ) ;
#12506 = CARTESIAN_POINT ( 'NONE',  ( -0.6814780602828901523, -1.267001069680700365, 48.72478509528001922 ) ) ;
#12507 = FACE_OUTER_BOUND ( 'NONE', #22174, .T. ) ;
#12508 = CARTESIAN_POINT ( 'NONE',  ( -15.62726112422596714, -28.45046755804883531, -2.999999999999971578 ) ) ;
#12509 = ORIENTED_EDGE ( 'NONE', *, *, #14724, .T. ) ;
#12510 = DIRECTION ( 'NONE',  ( -1.000000000000000000, -1.266830946243004623E-16, -4.336808689942002810E-19 ) ) ;
#12511 = ORIENTED_EDGE ( 'NONE', *, *, #22531, .T. ) ;
#12512 = CARTESIAN_POINT ( 'NONE',  ( -19.05255888325749325, 10.99999999999967670, -2.999999999999975131 ) ) ;
#12513 = CARTESIAN_POINT ( 'NONE',  ( -6.775203351379203376, 38.82189279864962117, 55.41163305959242535 ) ) ;
#12514 = CARTESIAN_POINT ( 'NONE',  ( 3.849727973822423851E-15, 1.500000000000011768, 0.000000000000000000 ) ) ;
#12515 = DIRECTION ( 'NONE',  ( 6.505213034913038160E-19, 3.903127820947822896E-18, 1.000000000000000000 ) ) ;
#12516 = CYLINDRICAL_SURFACE ( 'NONE', #4301, 19.11328065563151668 ) ;
#12517 = ADVANCED_FACE ( 'NONE', ( #10407 ), #18059, .T. ) ;
#12518 = CARTESIAN_POINT ( 'NONE',  ( 19.88513910325152523, 17.69449494136076950, 58.11726460477455447 ) ) ;
#12519 = DIRECTION ( 'NONE',  ( 6.505213034913038160E-19, 3.903127820947822896E-18, 1.000000000000000000 ) ) ;
#12520 = AXIS2_PLACEMENT_3D ( 'NONE', #9248, #3882, #10729 ) ;
#12521 = VECTOR ( 'NONE', #12205, 1000.000000000000000 ) ;
#12522 = CARTESIAN_POINT ( 'NONE',  ( 27.56232195404068008, -21.41958700883258970, 2.999999999999995559 ) ) ;
#12523 = EDGE_CURVE ( 'NONE', #1500, #11550, #21740, .T. ) ;
#12524 = EDGE_CURVE ( 'NONE', #13542, #2593, #17324, .T. ) ;
#12525 = AXIS2_PLACEMENT_3D ( 'NONE', #17352, #22532, #6827 ) ;
#12527 = EDGE_CURVE ( 'NONE', #3040, #3905, #20520, .T. ) ;
#12526 = VERTEX_POINT ( 'NONE', #12248 ) ;
#12528 = ORIENTED_EDGE ( 'NONE', *, *, #13320, .T. ) ;
#12529 = ORIENTED_EDGE ( 'NONE', *, *, #17997, .T. ) ;
#12530 = ORIENTED_EDGE ( 'NONE', *, *, #22654, .F. ) ;
#12531 = DIRECTION ( 'NONE',  ( -0.000000000000000000, 1.000000000000000000, -0.000000000000000000 ) ) ;
#12532 = CARTESIAN_POINT ( 'NONE',  ( -35.00000000000000000, 14.00000000000000000, 2.365113165210053967E-14 ) ) ;
#12533 = CARTESIAN_POINT ( 'NONE',  ( -4.918774254215691144, 31.11359284679368642, 3.000000000000023537 ) ) ;
#12534 = EDGE_CURVE ( 'NONE', #8936, #17952, #13646, .T. ) ;
#12535 = DIRECTION ( 'NONE',  ( -0.000000000000000000, 1.000000000000000000, -0.000000000000000000 ) ) ;
#12536 = CARTESIAN_POINT ( 'NONE',  ( 0.4769526114005525619, 39.99865964525184125, 49.10162959029930363 ) ) ;
#12537 = VECTOR ( 'NONE', #19727, 1000.000000000000000 ) ;
#12538 = VECTOR ( 'NONE', #11647, 1000.000000000000000 ) ;
#12539 = EDGE_LOOP ( 'NONE', ( #18420, #13334, #12175, #3187 ) ) ;
#12540 = DIRECTION ( 'NONE',  ( 6.505213034913038160E-19, 3.903127820947822896E-18, 1.000000000000000000 ) ) ;
#12541 = CARTESIAN_POINT ( 'NONE',  ( 35.00000000000058265, 26.00000000000000355, -57.10000000000076170 ) ) ;
#12542 = PRODUCT_DEFINITION_CONTEXT ( 'detailed design', #16165, 'design' ) ;
#12543 = FACE_OUTER_BOUND ( 'NONE', #11740, .T. ) ;
#12544 = CARTESIAN_POINT ( 'NONE',  ( -1.387778780781445518E-14, 20.00000000000000355, 102.0000000000000142 ) ) ;
#12545 = CARTESIAN_POINT ( 'NONE',  ( -35.00000000000000000, -9.000000000000001776, 18.00000000000001421 ) ) ;
#12546 = AXIS2_PLACEMENT_3D ( 'NONE', #19399, #9865, #21792 ) ;
#12547 = FACE_OUTER_BOUND ( 'NONE', #6293, .T. ) ;
#12548 = FACE_OUTER_BOUND ( 'NONE', #2310, .T. ) ;
#12549 = AXIS2_PLACEMENT_3D ( 'NONE', #6022, #14605, #2357 ) ;
#12550 = DIRECTION ( 'NONE',  ( 0.000000000000000000, 0.000000000000000000, -1.000000000000000000 ) ) ;
#12551 = ORIENTED_EDGE ( 'NONE', *, *, #13949, .T. ) ;
#12552 = AXIS2_PLACEMENT_3D ( 'NONE', #14363, #631, #10819 ) ;
#12553 = ORIENTED_EDGE ( 'NONE', *, *, #17946, .T. ) ;
#12554 = AXIS2_PLACEMENT_3D ( 'NONE', #11694, #1046, #9964 ) ;
#12555 = EDGE_CURVE ( 'NONE', #16284, #5849, #3797, .T. ) ;
#12556 = ORIENTED_EDGE ( 'NONE', *, *, #5405, .F. ) ;
#12557 = EDGE_CURVE ( 'NONE', #15629, #22134, #6722, .T. ) ;
#12558 = CARTESIAN_POINT ( 'NONE',  ( 12.15643230334913660, 40.00000000000000711, -54.39836425128640940 ) ) ;
#12559 = SPHERICAL_SURFACE ( 'NONE', #10247, 43.25806096964027603 ) ;
#12560 = AXIS2_PLACEMENT_3D ( 'NONE', #2944, #20688, #11977 ) ;
#12561 = CARTESIAN_POINT ( 'NONE',  ( 20.05817253550624457, -29.32895111104220831, -2.999999999999998224 ) ) ;
#12562 = EDGE_CURVE ( 'NONE', #17863, #18194, #21005, .T. ) ;
#12563 = DIRECTION ( 'NONE',  ( 0.7071067811865426878, 0.000000000000000000, 0.7071067811865524577 ) ) ;
#12564 = CARTESIAN_POINT ( 'NONE',  ( -16.97539716422060962, 9.395639044392956052, 59.81372721910508972 ) ) ;
#12565 = CARTESIAN_POINT ( 'NONE',  ( -15.91596560756144996, 32.12719615765574588, -56.91747558600052059 ) ) ;
#12566 = CARTESIAN_POINT ( 'NONE',  ( 2.775557561562891351E-14, -2.775557561562891351E-14, 2.999999999999999112 ) ) ;
#12567 = VECTOR ( 'NONE', #10963, 1000.000000000000000 ) ;
#12568 = ORIENTED_EDGE ( 'NONE', *, *, #5444, .F. ) ;
#12569 =( LENGTH_UNIT ( ) NAMED_UNIT ( * ) SI_UNIT ( .MILLI., .METRE. ) );
#12570 = B_SPLINE_CURVE_WITH_KNOTS ( 'NONE', 3,
 ( #1174, #15023, #952, #16647, #9775, #7948, #6229, #13294, #14909, #16877, #22041, #18361, #2681, #21935, #6334, #13189, #20324, #1075 ),
 .UNSPECIFIED., .F., .F.,
 ( 4, 2, 2, 2, 2, 2, 2, 2, 4 ),
 ( -3.543127106801270167E-05, 0.0006851204654910545561, 0.001405672202050121814, 0.002846775675168256546, 0.005728982621404526444, 0.007170086094522653587, 0.008611189567640779863, 0.01005229304075890701, 0.01149339651387703241 ),
 .UNSPECIFIED. ) ;
#12571 = DIRECTION ( 'NONE',  ( -1.000000000000000000, 2.831715466623964737E-14, 0.000000000000000000 ) ) ;
#12572 = DIRECTION ( 'NONE',  ( 1.000000000000000000, 0.000000000000000000, -1.224646799147353207E-16 ) ) ;
#12573 = ORIENTED_EDGE ( 'NONE', *, *, #20055, .F. ) ;
#12574 = DIRECTION ( 'NONE',  ( 6.505213034913038160E-19, 3.903127820947822896E-18, 1.000000000000000000 ) ) ;
#12575 = FACE_OUTER_BOUND ( 'NONE', #3067, .T. ) ;
#12576 = CARTESIAN_POINT ( 'NONE',  ( -1.387778780781445676E-14, 20.00000000000000000, -102.0000000000000142 ) ) ;
#12577 = EDGE_CURVE ( 'NONE', #10039, #7531, #18762, .T. ) ;
#12578 = AXIS2_PLACEMENT_3D ( 'NONE', #17867, #21305, #9157 ) ;
#12579 = VERTEX_POINT ( 'NONE', #1723 ) ;
#12580 = CIRCLE ( 'NONE', #19156, 2.500000000000002220 ) ;
#12581 = ORIENTED_EDGE ( 'NONE', *, *, #3412, .F. ) ;
#12582 = CARTESIAN_POINT ( 'NONE',  ( 1.387778780781445676E-14, -3.999999999999985345, -48.73397172404115452 ) ) ;
#12583 = CARTESIAN_POINT ( 'NONE',  ( -31.11359284679367221, -4.918774254215884767, 2.999999999999995559 ) ) ;
#12584 = CARTESIAN_POINT ( 'NONE',  ( -18.00000000000001421, 20.00000000000000355, -105.0000000000000142 ) ) ;
#12585 = ORIENTED_EDGE ( 'NONE', *, *, #16592, .F. ) ;
#12586 = LINE ( 'NONE', #3910, #12537 ) ;
#12587 = CARTESIAN_POINT ( 'NONE',  ( -1.387778780781445518E-14, 20.00000000000000355, 102.0000000000000142 ) ) ;
#12588 = VERTEX_POINT ( 'NONE', #20863 ) ;
#12589 = CARTESIAN_POINT ( 'NONE',  ( -5.999999999999999112, 0.000000000000000000, 6.000000000000001776 ) ) ;
#12590 = FACE_OUTER_BOUND ( 'NONE', #10588, .T. ) ;
#12591 = DIRECTION ( 'NONE',  ( 0.000000000000000000, -1.000000000000000000, 0.000000000000000000 ) ) ;
#12592 = CARTESIAN_POINT ( 'NONE',  ( -11.31876324338271544, -30.07487443287981677, -2.999999999999995559 ) ) ;
#12593 = ORIENTED_EDGE ( 'NONE', *, *, #13949, .F. ) ;
#12594 = CARTESIAN_POINT ( 'NONE',  ( -35.00000000000000000, 2.142135623730931471, -49.99999999999998579 ) ) ;
#12595 = AXIS2_PLACEMENT_3D ( 'NONE', #20383, #11667, #4906 ) ;
#12596 = LINE ( 'NONE', #19841, #154 ) ;
#12597 = CARTESIAN_POINT ( 'NONE',  ( -5.466611548547432697, 39.81233001754419121, -52.49274982270507195 ) ) ;
#12598 = EDGE_CURVE ( 'NONE', #12403, #19421, #14384, .T. ) ;
#12599 = VERTEX_POINT ( 'NONE', #20971 ) ;
#12600 = DIRECTION ( 'NONE',  ( 1.000000000000000000, 0.000000000000000000, 0.000000000000000000 ) ) ;
#12601 = CARTESIAN_POINT ( 'NONE',  ( 24.75236754129178607, 27.84804035626017793, -7.000000000000006217 ) ) ;
#12602 = CARTESIAN_POINT ( 'NONE',  ( -1.243967489023287243, -3.506377588453899790E-14, 51.43875557960417666 ) ) ;
#12603 = ADVANCED_FACE ( 'NONE', ( #4121 ), #10863, .T. ) ;
#12604 = EDGE_CURVE ( 'NONE', #2472, #15828, #10629, .T. ) ;
#12605 = AXIS2_PLACEMENT_3D ( 'NONE', #18149, #2686, #2462 ) ;
#12606 = ORIENTED_EDGE ( 'NONE', *, *, #73, .T. ) ;
#12607 = CIRCLE ( 'NONE', #7892, 22.00000000000000000 ) ;
#12608 = ORIENTED_EDGE ( 'NONE', *, *, #15182, .F. ) ;
#12609 = ORIENTED_EDGE ( 'NONE', *, *, #11870, .F. ) ;
#12610 = VERTEX_POINT ( 'NONE', #9266 ) ;
#12611 = DIRECTION ( 'NONE',  ( 1.000000000000000000, 0.000000000000000000, 0.000000000000000000 ) ) ;
#12612 = AXIS2_PLACEMENT_3D ( 'NONE', #22180, #2818, #13323 ) ;
#12613 = CARTESIAN_POINT ( 'NONE',  ( -32.10132595304128245, -5.074925817841801745, -6.999999999999999112 ) ) ;
#12614 = EDGE_CURVE ( 'NONE', #16628, #14700, #22468, .T. ) ;
#12615 = EDGE_LOOP ( 'NONE', ( #9984, #5592, #5171, #18005 ) ) ;
#12616 = DIRECTION ( 'NONE',  ( -6.505213034913038160E-19, -3.903127820947822896E-18, -1.000000000000000000 ) ) ;
#12617 = DIRECTION ( 'NONE',  ( -0.000000000000000000, -1.000000000000000000, -0.000000000000000000 ) ) ;
#12618 = EDGE_LOOP ( 'NONE', ( #10608, #17915, #2412, #18713 ) ) ;
#12619 = CARTESIAN_POINT ( 'NONE',  ( -2.999999999999999112, 30.00000000000000000, 6.485281374238567764 ) ) ;
#12620 = CARTESIAN_POINT ( 'NONE',  ( -22.41556111754674063, 20.62010838399689305, -58.66542762804073163 ) ) ;
#12621 = DIRECTION ( 'NONE',  ( 6.505213034913038160E-19, 3.903127820947822896E-18, 1.000000000000000000 ) ) ;
#12622 = ORIENTED_EDGE ( 'NONE', *, *, #19638, .T. ) ;
#12623 = CARTESIAN_POINT ( 'NONE',  ( 2.517875701374014508, 0.1458803431926766758, 52.33410116371960896 ) ) ;
#12624 = ORIENTED_EDGE ( 'NONE', *, *, #190, .T. ) ;
#12625 = DIRECTION ( 'NONE',  ( 8.659560562354902043E-17, -0.7071067811865500152, 0.7071067811865450192 ) ) ;
#12626 = AXIS2_PLACEMENT_3D ( 'NONE', #16051, #14320, #12488 ) ;
#12627 = ADVANCED_FACE ( 'NONE', ( #12575 ), #7094, .T. ) ;
#12628 = CARTESIAN_POINT ( 'NONE',  ( 3.849727973822423851E-15, 1.500000000000011768, 0.000000000000000000 ) ) ;
#12629 = DIRECTION ( 'NONE',  ( -1.000000000000000000, 0.000000000000000000, 0.000000000000000000 ) ) ;
#12630 = CARTESIAN_POINT ( 'NONE',  ( 1.247275002120749043, 0.02903096490061087345, 51.42826582519167999 ) ) ;
#12631 = AXIS2_PLACEMENT_3D ( 'NONE', #20011, #18285, #2363 ) ;
#12632 = ORIENTED_EDGE ( 'NONE', *, *, #3453, .F. ) ;
#12633 = CARTESIAN_POINT ( 'NONE',  ( 21.72501817863376061, 25.59362490671916390, 58.51313831023582424 ) ) ;
#12634 = DIRECTION ( 'NONE',  ( -0.000000000000000000, 1.000000000000000000, -0.000000000000000000 ) ) ;
#12635 = EDGE_CURVE ( 'NONE', #9318, #18860, #7453, .T. ) ;
#12636 = CIRCLE ( 'NONE', #3140, 2.499999999999995115 ) ;
#12637 = FACE_OUTER_BOUND ( 'NONE', #8812, .T. ) ;
#12638 = ORIENTED_EDGE ( 'NONE', *, *, #8578, .F. ) ;
#12639 = EDGE_LOOP ( 'NONE', ( #20338, #21885, #2401, #161, #16858, #6666 ) ) ;
#12640 =( BOUNDED_SURFACE ( )  B_SPLINE_SURFACE ( 3, 2, ( 
 ( #7499, #3842, #5662 ),
 ( #18267, #2117, #2578 ),
 ( #7727, #9108, #19654 ),
 ( #3960, #10928, #14472 ),
 ( #4075, #14698, #21708 ),
 ( #13307, #18721, #11386 ),
 ( #15031, #20448, #15375 ),
 ( #4857, #2804, #13537 ),
 ( #10109, #9897, #16885 ),
 ( #1182, #21946, #3136 ),
 ( #4639, #1417, #11726 ),
 ( #18613, #8292, #11504 ),
 ( #22163, #3025, #11828 ),
 ( #1084, #6462, #9994 ),
 ( #9783, #18372, #15143 ),
 ( #22284, #8179, #16657 ),
 ( #16778, #6344, #8074 ),
 ( #964, #22050, #18831 ),
 ( #22392, #13423, #20218 ),
 ( #4755, #16988, #1296 ),
 ( #20332, #13090, #7959 ),
 ( #14923, #15260, #17101 ),
 ( #6577, #8403, #2690 ),
 ( #9669, #20555, #6239 ),
 ( #11615, #20107, #4413 ),
 ( #2923, #13197, #4522 ),
 ( #18489, #14293, #9269 ),
 ( #21416, #19059, #7435 ),
 ( #4020, #3781, #10744 ),
 ( #4967, #12694, #11950 ),
 ( #18948, #15599, #16130 ),
 ( #22504, #19715, #17748 ) ),
 .UNSPECIFIED., .F., .F., .F. ) 
 B_SPLINE_SURFACE_WITH_KNOTS ( ( 4, 2, 2, 2, 2, 2, 2, 2, 2, 2, 2, 2, 2, 2, 2, 4 ),
 ( 3, 3 ),
 ( 0.000000000000000000, 0.005810029919203046553, 0.008715044878804568962, 0.01162005983840609311, 0.01452507479800761551, 0.01743008975760913792, 0.02033510471721066207, 0.02324011967681218621, 0.02614513463641370689, 0.02905014959601523103, 0.03486017951521827585, 0.03631268699501903618, 0.03776519447481979652, 0.04067020943442132414, 0.04357522439402285175, 0.04648023935362437242 ),
 ( 0.000000000000000000, 1.000000000000000000 ),
 .UNSPECIFIED. ) 
 GEOMETRIC_REPRESENTATION_ITEM ( )  RATIONAL_B_SPLINE_SURFACE ( (
 ( 1.000000000000000000, 0.6428092274089103331, 1.000000000000000000),
 ( 1.000000000000000000, 0.6349692141176793703, 1.000000000000000000),
 ( 1.000000000000000000, 0.6297610438357627016, 1.000000000000000000),
 ( 1.000000000000000000, 0.6250724677584068578, 1.000000000000000000),
 ( 1.000000000000000000, 0.6240291009521173882, 1.000000000000000000),
 ( 1.000000000000000000, 0.6228114827670524489, 1.000000000000000000),
 ( 1.000000000000000000, 0.6226217323249612079, 1.000000000000000000),
 ( 1.000000000000000000, 0.6227877533346650729, 1.000000000000000000),
 ( 1.000000000000000000, 0.6231437405070447966, 1.000000000000000000),
 ( 1.000000000000000000, 0.6241327156850213775, 1.000000000000000000),
 ( 1.000000000000000000, 0.6247528374326117850, 1.000000000000000000),
 ( 1.000000000000000000, 0.6259854008239856826, 1.000000000000000000),
 ( 1.000000000000000000, 0.6265990906519964820, 1.000000000000000000),
 ( 1.000000000000000000, 0.6276348137186016363, 1.000000000000000000),
 ( 1.000000000000000000, 0.6280565648738838380, 1.000000000000000000),
 ( 1.000000000000000000, 0.6285705475686420574, 1.000000000000000000),
 ( 1.000000000000000000, 0.6286676444210588244, 1.000000000000000000),
 ( 1.000000000000000000, 0.6285219413506923924, 1.000000000000000000),
 ( 1.000000000000000000, 0.6282782847648648028, 1.000000000000000000),
 ( 1.000000000000000000, 0.6271139948487377547, 1.000000000000000000),
 ( 1.000000000000000000, 0.6257653971627769041, 1.000000000000000000),
 ( 1.000000000000000000, 0.6242767683747761920, 1.000000000000000000),
 ( 1.000000000000000000, 0.6239908339052062658, 1.000000000000000000),
 ( 1.000000000000000000, 0.6234800620773224278, 1.000000000000000000),
 ( 1.000000000000000000, 0.6232570855785173336, 1.000000000000000000),
 ( 1.000000000000000000, 0.6227348070526912416, 1.000000000000000000),
 ( 1.000000000000000000, 0.6225812994807357059, 1.000000000000000000),
 ( 1.000000000000000000, 0.6229454059011351186, 1.000000000000000000),
 ( 1.000000000000000000, 0.6234652178689191748, 1.000000000000000000),
 ( 1.000000000000000000, 0.6254772350198137820, 1.000000000000000000),
 ( 1.000000000000000000, 0.6269570472270592498, 1.000000000000000000),
 ( 1.000000000000000000, 0.6290213284793358950, 1.000000000000000000) ) ) 
 REPRESENTATION_ITEM ( '' )  SURFACE ( )  );
#12641 = EDGE_LOOP ( 'NONE', ( #4850, #11402, #13543, #8923 ) ) ;
#12642 = CONICAL_SURFACE ( 'NONE', #201, 2.099999999999990763, 1.029744258676652091 ) ;
#12643 = ORIENTED_EDGE ( 'NONE', *, *, #9082, .T. ) ;
#12644 = CYLINDRICAL_SURFACE ( 'NONE', #442, 6.499999999999999112 ) ;
#12645 = CARTESIAN_POINT ( 'NONE',  ( -42.50000000000000711, -5.000000000000000000, 47.50000000000000711 ) ) ;
#12646 = CIRCLE ( 'NONE', #16326, 19.11328065563151668 ) ;
#12647 = DIRECTION ( 'NONE',  ( 1.296372316667914327E-16, 1.000000000000000000, -0.000000000000000000 ) ) ;
#12648 = ADVANCED_FACE ( 'NONE', ( #14526 ), #19903, .T. ) ;
#12649 = ORIENTED_EDGE ( 'NONE', *, *, #18562, .F. ) ;
#12650 = LINE ( 'NONE', #755, #9478 ) ;
#12651 = FACE_OUTER_BOUND ( 'NONE', #22252, .T. ) ;
#12652 = CIRCLE ( 'NONE', #7914, 34.00000000000000000 ) ;
#12653 = ORIENTED_EDGE ( 'NONE', *, *, #13130, .T. ) ;
#12654 = CARTESIAN_POINT ( 'NONE',  ( 47.83731665821558465, 10.00000000000000000, 38.93845529828710994 ) ) ;
#12655 = LINE ( 'NONE', #21159, #20801 ) ;
#12656 = EDGE_CURVE ( 'NONE', #7389, #1702, #12931, .T. ) ;
#12657 = DIRECTION ( 'NONE',  ( -0.000000000000000000, 1.000000000000000000, -0.000000000000000000 ) ) ;
#12658 = CARTESIAN_POINT ( 'NONE',  ( -19.98183132229268466, 20.98212305896295504, -60.61750244562276890 ) ) ;
#12659 = DIRECTION ( 'NONE',  ( 1.000000000000000000, 0.000000000000000000, 0.000000000000000000 ) ) ;
#12660 = CIRCLE ( 'NONE', #15591, 18.00000000000000000 ) ;
#12661 = VECTOR ( 'NONE', #3064, 1000.000000000000000 ) ;
#12662 = AXIS2_PLACEMENT_3D ( 'NONE', #19166, #24, #21105 ) ;
#12663 = LINE ( 'NONE', #9479, #11489 ) ;
#12664 = CARTESIAN_POINT ( 'NONE',  ( -8.485281374238560659, 28.19616000222403684, 3.000000000000000000 ) ) ;
#12665 = EDGE_CURVE ( 'NONE', #16393, #10093, #7548, .T. ) ;
#12666 = VERTEX_POINT ( 'NONE', #101 ) ;
#12667 = CIRCLE ( 'NONE', #6838, 10.00000000000000178 ) ;
#12668 = ORIENTED_EDGE ( 'NONE', *, *, #6519, .T. ) ;
#12669 = ORIENTED_EDGE ( 'NONE', *, *, #1320, .F. ) ;
#12670 = DIRECTION ( 'NONE',  ( -1.296372316667914327E-16, -1.000000000000000000, 0.000000000000000000 ) ) ;
#12671 = EDGE_CURVE ( 'NONE', #7232, #14245, #21415, .T. ) ;
#12672 = DIRECTION ( 'NONE',  ( 0.000000000000000000, -0.000000000000000000, -1.000000000000000000 ) ) ;
#12673 = CARTESIAN_POINT ( 'NONE',  ( -34.24928931925764886, 6.742883674876548383, 2.999999999999999112 ) ) ;
#12674 = DIRECTION ( 'NONE',  ( -0.000000000000000000, -1.000000000000000000, -0.000000000000000000 ) ) ;
#12675 = DIRECTION ( 'NONE',  ( 0.000000000000000000, -0.000000000000000000, 1.000000000000000000 ) ) ;
#12676 = FACE_OUTER_BOUND ( 'NONE', #14268, .T. ) ;
#12677 = CARTESIAN_POINT ( 'NONE',  ( -9.081037608035938291, 37.83854577724346768, -56.73868670302932316 ) ) ;
#12678 = DIRECTION ( 'NONE',  ( 1.000000000000000000, 0.000000000000000000, 0.000000000000000000 ) ) ;
#12679 = CIRCLE ( 'NONE', #18869, 2.499999999999998668 ) ;
#12680 = VERTEX_POINT ( 'NONE', #1939 ) ;
#12681 = LINE ( 'NONE', #17856, #14142 ) ;
#12682 = CARTESIAN_POINT ( 'NONE',  ( -42.50000000000000711, -12.00000000000000000, -45.00000000000000000 ) ) ;
#12683 = CARTESIAN_POINT ( 'NONE',  ( -22.15900668633775794, -29.33526866242097597, 2.800654218530509443 ) ) ;
#12684 = PLANE ( 'NONE',  #169 ) ;
#12685 = CARTESIAN_POINT ( 'NONE',  ( -27.19760187735852242, -24.73600648735135721, 2.800654218530492123 ) ) ;
#12686 = EDGE_CURVE ( 'NONE', #22510, #15748, #14060, .T. ) ;
#12687 = ORIENTED_EDGE ( 'NONE', *, *, #16315, .F. ) ;
#12688 = EDGE_CURVE ( 'NONE', #13845, #3722, #211, .T. ) ;
#12689 = ORIENTED_EDGE ( 'NONE', *, *, #1448, .F. ) ;
#12690 = FACE_OUTER_BOUND ( 'NONE', #8334, .T. ) ;
#12691 = AXIS2_PLACEMENT_3D ( 'NONE', #2216, #16296, #607 ) ;
#12692 = DIRECTION ( 'NONE',  ( 0.000000000000000000, -0.000000000000000000, -1.000000000000000000 ) ) ;
#12693 = CIRCLE ( 'NONE', #20763, 2.500000000000002220 ) ;
#12694 = CARTESIAN_POINT ( 'NONE',  ( 13.52717286024270216, 5.231573370292008640, -56.05142967219527605 ) ) ;
#12695 = ADVANCED_FACE ( 'NONE', ( #4019 ), #12805, .F. ) ;
#12696 = EDGE_LOOP ( 'NONE', ( #22417, #12784, #8369, #12397 ) ) ;
#12697 = CARTESIAN_POINT ( 'NONE',  ( -16.99647590252638452, -30.48934413892778750, 2.999999999999999112 ) ) ;
#12698 = AXIS2_PLACEMENT_3D ( 'NONE', #6438, #13401, #11924 ) ;
#12699 = AXIS2_PLACEMENT_3D ( 'NONE', #5876, #14330, #5759 ) ;
#12700 = ORIENTED_EDGE ( 'NONE', *, *, #16396, .T. ) ;
#12701 = VECTOR ( 'NONE', #13284, 1000.000000000000000 ) ;
#12702 = DIRECTION ( 'NONE',  ( 1.296372316667914327E-16, 1.000000000000000000, -0.000000000000000000 ) ) ;
#12703 = DIRECTION ( 'NONE',  ( -1.000000000000000000, -1.208970125616060101E-17, 6.505213034913038160E-19 ) ) ;
#12704 = CIRCLE ( 'NONE', #2858, 2.500000000000002220 ) ;
#12705 = VERTEX_POINT ( 'NONE', #16129 ) ;
#12706 = CYLINDRICAL_SURFACE ( 'NONE', #18771, 36.76383501243555685 ) ;
#12707 = CARTESIAN_POINT ( 'NONE',  ( -9.433062738409624615, 40.00000000000000711, 53.48670742531720634 ) ) ;
#12708 = ORIENTED_EDGE ( 'NONE', *, *, #8400, .T. ) ;
#12709 = CARTESIAN_POINT ( 'NONE',  ( -22.15900668633775794, -29.33526866242097597, 2.800654218530509443 ) ) ;
#12710 = CARTESIAN_POINT ( 'NONE',  ( -22.00000000000001421, 20.00000000000000000, -98.00000000000000000 ) ) ;
#12711 = CIRCLE ( 'NONE', #7227, 2.524999999999999467 ) ;
#12712 = FACE_OUTER_BOUND ( 'NONE', #13852, .T. ) ;
#12713 = CARTESIAN_POINT ( 'NONE',  ( -34.74700806321097701, 12.00937115242647835, -2.000000000000001776 ) ) ;
#12714 = EDGE_LOOP ( 'NONE', ( #9891, #12909 ) ) ;
#12715 = CARTESIAN_POINT ( 'NONE',  ( -35.00000000000000000, -4.999999999999997335, 1.387778780781445676E-14 ) ) ;
#12716 = CARTESIAN_POINT ( 'NONE',  ( -1.128083539116253586, -34.88850421923977763, -2.999999999999971578 ) ) ;
#12717 = FACE_OUTER_BOUND ( 'NONE', #9342, .T. ) ;
#12718 = ADVANCED_FACE ( 'NONE', ( #21193 ), #10466, .F. ) ;
#12719 = VERTEX_POINT ( 'NONE', #12462 ) ;
#12720 = CIRCLE ( 'NONE', #660, 31.50000000000000711 ) ;
#12721 = CARTESIAN_POINT ( 'NONE',  ( -12.48541242016036179, 28.32175387455462712, 44.64471390988171606 ) ) ;
#12722 = CARTESIAN_POINT ( 'NONE',  ( 35.00000000000000000, 17.00000000000000000, 2.365113165210053967E-14 ) ) ;
#12723 = CIRCLE ( 'NONE', #21525, 36.76383501243555685 ) ;
#12724 = AXIS2_PLACEMENT_3D ( 'NONE', #4587, #6530, #2645 ) ;
#12725 = EDGE_CURVE ( 'NONE', #11771, #11765, #19992, .T. ) ;
#12726 = VECTOR ( 'NONE', #7854, 1000.000000000000000 ) ;
#12727 = VECTOR ( 'NONE', #13281, 1000.000000000000000 ) ;
#12728 = ORIENTED_EDGE ( 'NONE', *, *, #16769, .F. ) ;
#12729 = ORIENTED_EDGE ( 'NONE', *, *, #13506, .F. ) ;
#12730 = EDGE_LOOP ( 'NONE', ( #16929, #5552, #8043, #8269 ) ) ;
#12731 = SHAPE_REPRESENTATION_RELATIONSHIP ( 'NONE' , 'NONE' ,  #13507, #4987 ) ;
#12732 = ADVANCED_FACE ( 'NONE', ( #21304, #16249 ), #16021, .F. ) ;
#12733 = EDGE_LOOP ( 'NONE', ( #11447, #10025, #19904, #1554 ) ) ;
#12734 = CARTESIAN_POINT ( 'NONE',  ( -0.6841746959065087008, -36.75746821813308429, -2.000000000000005329 ) ) ;
#12735 = CARTESIAN_POINT ( 'NONE',  ( 2.777950727038989154, 39.99999999999999289, -50.42550754305786853 ) ) ;
#12736 = CARTESIAN_POINT ( 'NONE',  ( -34.99999999999999289, -5.000000000000000000, -3.012171160963566127E-14 ) ) ;
#12737 = CIRCLE ( 'NONE', #18618, 9.000000000000035527 ) ;
#12738 = ORIENTED_EDGE ( 'NONE', *, *, #19008, .F. ) ;
#12739 = CARTESIAN_POINT ( 'NONE',  ( 35.00000000000001421, 1.000000000000044187, 10.00000000000000000 ) ) ;
#12740 = CARTESIAN_POINT ( 'NONE',  ( 21.65063509461093005, 12.50000000000006750, -5.000000000000004441 ) ) ;
#12741 = ORIENTED_EDGE ( 'NONE', *, *, #20125, .T. ) ;
#12742 = CARTESIAN_POINT ( 'NONE',  ( 19.59430950039339692, -28.88846368933353759, 3.000000000000023537 ) ) ;
#12743 = CARTESIAN_POINT ( 'NONE',  ( 0.000000000000000000, -1.500000000000015099, 11.99999999999985256 ) ) ;
#12744 = CIRCLE ( 'NONE', #21543, 2.099999999999997868 ) ;
#12745 = EDGE_CURVE ( 'NONE', #6428, #16050, #3542, .T. ) ;
#12746 = AXIS2_PLACEMENT_3D ( 'NONE', #19760, #18020, #18259 ) ;
#12747 = DIRECTION ( 'NONE',  ( -1.296372316667914327E-16, -1.000000000000000000, 0.000000000000000000 ) ) ;
#12748 = ORIENTED_EDGE ( 'NONE', *, *, #3032, .T. ) ;
#12749 = DIRECTION ( 'NONE',  ( 0.9659258262890680902, 0.2588190451025216832, 1.182917971378669349E-16 ) ) ;
#12750 = EDGE_LOOP ( 'NONE', ( #22679, #1050, #16270, #5752 ) ) ;
#12751 = CARTESIAN_POINT ( 'NONE',  ( 5.133442403747772609, 39.34078726959584316, 53.02546941656563462 ) ) ;
#12752 = DIRECTION ( 'NONE',  ( 0.000000000000000000, 0.000000000000000000, 1.000000000000000000 ) ) ;
#12753 = DIRECTION ( 'NONE',  ( 1.296372316667914327E-16, 1.000000000000000000, -0.000000000000000000 ) ) ;
#12754 = CYLINDRICAL_SURFACE ( 'NONE', #4523, 60.00000000000000000 ) ;
#12755 = ORIENTED_EDGE ( 'NONE', *, *, #975, .T. ) ;
#12756 = CARTESIAN_POINT ( 'NONE',  ( 21.22368364729369361, 12.66551901741837405, 58.39771426751187278 ) ) ;
#12757 = DIRECTION ( 'NONE',  ( -1.000000000000000000, 0.000000000000000000, 0.000000000000000000 ) ) ;
#12758 = FACE_BOUND ( 'NONE', #15467, .T. ) ;
#12759 = VECTOR ( 'NONE', #11810, 1000.000000000000000 ) ;
#12760 = ORIENTED_EDGE ( 'NONE', *, *, #10857, .F. ) ;
#12761 = ORIENTED_EDGE ( 'NONE', *, *, #10562, .F. ) ;
#12762 = ORIENTED_EDGE ( 'NONE', *, *, #13900, .T. ) ;
#12763 = EDGE_CURVE ( 'NONE', #1089, #17558, #10080, .T. ) ;
#12764 = AXIS2_PLACEMENT_3D ( 'NONE', #11473, #22477, #1611 ) ;
#12765 = ORIENTED_EDGE ( 'NONE', *, *, #20358, .F. ) ;
#12766 = CARTESIAN_POINT ( 'NONE',  ( 3.460816278822046447E-15, -1.500000000000011768, 0.000000000000000000 ) ) ;
#12767 = CARTESIAN_POINT ( 'NONE',  ( -11.25639079541607934, 39.09917355307971576, -55.11545576720666162 ) ) ;
#12768 = FACE_OUTER_BOUND ( 'NONE', #22663, .T. ) ;
#12769 = ORIENTED_EDGE ( 'NONE', *, *, #5252, .F. ) ;
#12770 = CARTESIAN_POINT ( 'NONE',  ( -0.7809641287213069383, -4.625293788889051072, 46.06432795380178646 ) ) ;
#12771 = ADVANCED_FACE ( 'NONE', ( #9721 ), #21996, .T. ) ;
#12772 = CIRCLE ( 'NONE', #2924, 19.99999999999999289 ) ;
#12773 = EDGE_LOOP ( 'NONE', ( #20450, #17105, #11863, #13074 ) ) ;
#12774 = DIRECTION ( 'NONE',  ( 0.000000000000000000, 0.000000000000000000, 1.000000000000000000 ) ) ;
#12775 = CARTESIAN_POINT ( 'NONE',  ( -42.50000000000000711, -12.00000000000000000, 47.50000000000000711 ) ) ;
#12776 = CARTESIAN_POINT ( 'NONE',  ( -31.57187188083505802, -7.711478842616608986, -2.999999999999971578 ) ) ;
#12777 = DIRECTION ( 'NONE',  ( -0.000000000000000000, -1.000000000000000000, -0.000000000000000000 ) ) ;
#12778 = DIRECTION ( 'NONE',  ( 0.000000000000000000, -0.000000000000000000, 1.000000000000000000 ) ) ;
#12779 = CARTESIAN_POINT ( 'NONE',  ( -1.485790755603442514E-14, 40.00000000000000000, 48.73397172404484223 ) ) ;
#12780 = EDGE_CURVE ( 'NONE', #10746, #22194, #9739, .T. ) ;
#12781 =( BOUNDED_SURFACE ( )  B_SPLINE_SURFACE ( 3, 2, ( 
 ( #5320, #19304, #10236 ),
 ( #17229, #1542, #14108 ),
 ( #17571, #22521, #8639 ),
 ( #20911, #13780, #486 ),
 ( #17796, #21346, #21463 ),
 ( #18135, #5766, #8969 ),
 ( #9434, #16175, #12506 ),
 ( #7483, #15951, #19757 ) ),
 .UNSPECIFIED., .F., .F., .F. ) 
 B_SPLINE_SURFACE_WITH_KNOTS ( ( 4, 2, 2, 4 ),
 ( 3, 3 ),
 ( 0.000000000000000000, 0.005621242337451588626, 0.008431863506177382506, 0.01124248467490317725 ),
 ( 0.000000000000000000, 1.000000000000000000 ),
 .UNSPECIFIED. ) 
 GEOMETRIC_REPRESENTATION_ITEM ( )  RATIONAL_B_SPLINE_SURFACE ( (
 ( 1.000000000000000000, 0.7200096751079151369, 1.000000000000000000),
 ( 1.000000000000000000, 0.7496970740839632441, 1.000000000000000000),
 ( 1.000000000000000000, 0.7737958965667965927, 1.000000000000000000),
 ( 1.000000000000000000, 0.8024469391899264892, 1.000000000000000000),
 ( 1.000000000000000000, 0.8107372619350866616, 1.000000000000000000),
 ( 1.000000000000000000, 0.8249110457735379098, 1.000000000000000000),
 ( 1.000000000000000000, 0.8307983230915116923, 1.000000000000000000),
 ( 1.000000000000000000, 0.8354958991656090683, 1.000000000000000000) ) ) 
 REPRESENTATION_ITEM ( '' )  SURFACE ( )  );
#12782 = DIRECTION ( 'NONE',  ( 0.000000000000000000, -1.000000000000000000, 0.000000000000000000 ) ) ;
#12783 = ORIENTED_EDGE ( 'NONE', *, *, #18581, .T. ) ;
#12784 = ORIENTED_EDGE ( 'NONE', *, *, #21089, .T. ) ;
#12785 = AXIS2_PLACEMENT_3D ( 'NONE', #17789, #2094, #21015 ) ;
#12786 = EDGE_CURVE ( 'NONE', #20078, #15733, #6826, .T. ) ;
#12787 = ORIENTED_EDGE ( 'NONE', *, *, #8470, .T. ) ;
#12788 = DIRECTION ( 'NONE',  ( -6.505213034913038160E-19, -3.903127820947822896E-18, -1.000000000000000000 ) ) ;
#12789 = DIRECTION ( 'NONE',  ( 6.505213034913038160E-19, 3.903127820947822896E-18, 1.000000000000000000 ) ) ;
#12790 = CARTESIAN_POINT ( 'NONE',  ( 7.538500903810520626, 38.52938254314626221, 55.92181088654620424 ) ) ;
#12791 = DIRECTION ( 'NONE',  ( 0.000000000000000000, 0.000000000000000000, -1.000000000000000000 ) ) ;
#12792 = CARTESIAN_POINT ( 'NONE',  ( -10.88890858922316163, 36.78121034548709645, -57.56873443368869658 ) ) ;
#12793 = CYLINDRICAL_SURFACE ( 'NONE', #10782, 2.999999999999999112 ) ;
#12794 = VECTOR ( 'NONE', #14679, 1000.000000000000000 ) ;
#12795 = ORIENTED_EDGE ( 'NONE', *, *, #13335, .T. ) ;
#12796 = DIRECTION ( 'NONE',  ( -0.000000000000000000, 1.000000000000000000, -0.000000000000000000 ) ) ;
#12797 = DIRECTION ( 'NONE',  ( 6.505213034913038160E-19, 3.903127820947822896E-18, 1.000000000000000000 ) ) ;
#12798 = DIRECTION ( 'NONE',  ( 1.296372316667914327E-16, 1.000000000000000000, -0.000000000000000000 ) ) ;
#12799 = CARTESIAN_POINT ( 'NONE',  ( -24.75236754129155159, -27.84804035626051189, 2.999999999999995559 ) ) ;
#12800 = VERTEX_POINT ( 'NONE', #18424 ) ;
#12801 = CARTESIAN_POINT ( 'NONE',  ( 2.220446049250313081E-13, -8.326672684688674053E-14, 2.800654218530498785 ) ) ;
#12802 = ORIENTED_EDGE ( 'NONE', *, *, #8958, .F. ) ;
#12803 = EDGE_CURVE ( 'NONE', #19609, #13854, #4234, .T. ) ;
#12804 = LINE ( 'NONE', #901, #1263 ) ;
#12805 = CYLINDRICAL_SURFACE ( 'NONE', #5714, 1.000000000000000888 ) ;
#12806 = EDGE_CURVE ( 'NONE', #11307, #8182, #14093, .T. ) ;
#12807 = EDGE_CURVE ( 'NONE', #9457, #21700, #2520, .T. ) ;
#12808 = ORIENTED_EDGE ( 'NONE', *, *, #14311, .F. ) ;
#12809 = FACE_OUTER_BOUND ( 'NONE', #7730, .T. ) ;
#12810 = CARTESIAN_POINT ( 'NONE',  ( 5.553314835777164227, 39.99999999999998579, -51.88330480362772335 ) ) ;
#12811 = EDGE_CURVE ( 'NONE', #9285, #4760, #22567, .T. ) ;
#12812 = ORIENTED_EDGE ( 'NONE', *, *, #11310, .T. ) ;
#12813 = CARTESIAN_POINT ( 'NONE',  ( 4.557463200991922037, 39.87073523829934629, -51.93758469931694322 ) ) ;
#12814 = CYLINDRICAL_SURFACE ( 'NONE', #372, 19.11328065563152379 ) ;
#12815 = FACE_OUTER_BOUND ( 'NONE', #13056, .T. ) ;
#12816 = EDGE_CURVE ( 'NONE', #15720, #14743, #12652, .T. ) ;
#12817 = EDGE_LOOP ( 'NONE', ( #5150, #18723 ) ) ;
#12818 = FACE_BOUND ( 'NONE', #3370, .T. ) ;
#12819 = DIRECTION ( 'NONE',  ( 1.000000000000000000, 0.000000000000000000, 0.000000000000000000 ) ) ;
#12820 = ORIENTED_EDGE ( 'NONE', *, *, #11671, .F. ) ;
#12821 = CARTESIAN_POINT ( 'NONE',  ( 35.00000000000000711, 0.000000000000000000, 49.99999999999999289 ) ) ;
#12822 = FACE_OUTER_BOUND ( 'NONE', #9309, .T. ) ;
#12823 = CARTESIAN_POINT ( 'NONE',  ( -8.194244601622644453, 39.99999999999999289, 53.04029799712058235 ) ) ;
#12824 = AXIS2_PLACEMENT_3D ( 'NONE', #8520, #19184, #19069 ) ;
#12825 = CARTESIAN_POINT ( 'NONE',  ( 42.50000000000000711, -5.000000000000000000, -47.50000000000000000 ) ) ;
#12826 = ORIENTED_EDGE ( 'NONE', *, *, #218, .F. ) ;
#12827 = CARTESIAN_POINT ( 'NONE',  ( -21.97438720605730822, 22.98755168577401520, -7.000000000000006217 ) ) ;
#12828 = DIRECTION ( 'NONE',  ( -0.9898477157360405787, 0.000000000000000000, 0.1421319796954322312 ) ) ;
#12829 = ORIENTED_EDGE ( 'NONE', *, *, #14501, .T. ) ;
#12830 = CARTESIAN_POINT ( 'NONE',  ( -12.68897045256290035, 28.00829229206842896, 44.74667050109238886 ) ) ;
#12831 = CARTESIAN_POINT ( 'NONE',  ( 13.56354382738800268, 2.142135623730931471, 56.03997097393685323 ) ) ;
#12832 = VECTOR ( 'NONE', #5175, 1000.000000000000000 ) ;
#12833 = ORIENTED_EDGE ( 'NONE', *, *, #10768, .T. ) ;
#12834 = ORIENTED_EDGE ( 'NONE', *, *, #9469, .T. ) ;
#12835 = ORIENTED_EDGE ( 'NONE', *, *, #7385, .F. ) ;
#12836 = CARTESIAN_POINT ( 'NONE',  ( 118.3948287847375127, 176.9344539442019197, -25.76723676782311756 ) ) ;
#12837 = EDGE_CURVE ( 'NONE', #5871, #20053, #14310, .T. ) ;
#12838 = VERTEX_POINT ( 'NONE', #20046 ) ;
#12839 = LINE ( 'NONE', #12734, #5917 ) ;
#12840 = CARTESIAN_POINT ( 'NONE',  ( 35.00000000000000000, -5.000000000000000000, 52.49999999999698019 ) ) ;
#12841 = CARTESIAN_POINT ( 'NONE',  ( 3.182708703124521588, 40.00000000000000711, -50.65274029778007048 ) ) ;
#12842 = ADVANCED_FACE ( 'NONE', ( #13145 ), #18316, .F. ) ;
#12843 = DIRECTION ( 'NONE',  ( 0.000000000000000000, 1.000000000000000000, 0.000000000000000000 ) ) ;
#12844 = CARTESIAN_POINT ( 'NONE',  ( 31.57187188083543461, 7.711478842616415363, 2.999999999999995559 ) ) ;
#12845 = ORIENTED_EDGE ( 'NONE', *, *, #14145, .F. ) ;
#12846 = CARTESIAN_POINT ( 'NONE',  ( -20.55056392469585802, 29.75120097320018431, -2.932164912090549969 ) ) ;
#12847 = CARTESIAN_POINT ( 'NONE',  ( -3.999999999999996447, 1.499999999999994893, 0.000000000000000000 ) ) ;
#12848 = VERTEX_POINT ( 'NONE', #6399 ) ;
#12849 = CARTESIAN_POINT ( 'NONE',  ( 2.220446049250313081E-13, -8.326672684688674053E-14, 2.800654218530498785 ) ) ;
#12850 = CARTESIAN_POINT ( 'NONE',  ( -17.68664055422813774, 6.162676607241205140, -57.44855069909471013 ) ) ;
#12851 = CIRCLE ( 'NONE', #9933, 2.500000000000002220 ) ;
#12852 = CARTESIAN_POINT ( 'NONE',  ( 28.45046755804903071, -15.62726112422607727, 3.000000000000023537 ) ) ;
#12853 = ORIENTED_EDGE ( 'NONE', *, *, #11414, .T. ) ;
#12854 = CARTESIAN_POINT ( 'NONE',  ( 35.00000000000001421, 0.000000000000000000, -4.999999999999997335 ) ) ;
#12855 = EDGE_CURVE ( 'NONE', #22631, #5849, #4355, .T. ) ;
#12856 = VERTEX_POINT ( 'NONE', #9606 ) ;
#12857 = CARTESIAN_POINT ( 'NONE',  ( 1.268121568163981028, 39.97056933375354504, 50.22305475356784399 ) ) ;
#12858 = CYLINDRICAL_SURFACE ( 'NONE', #20846, 2.500000000000002220 ) ;
#12859 = DIRECTION ( 'NONE',  ( 0.000000000000000000, 0.000000000000000000, -1.000000000000000000 ) ) ;
#12860 = ORIENTED_EDGE ( 'NONE', *, *, #11175, .F. ) ;
#12861 = LINE ( 'NONE', #6002, #16738 ) ;
#12862 = PLANE ( 'NONE',  #12605 ) ;
#12863 = CARTESIAN_POINT ( 'NONE',  ( 15.50000000000024336, -2.516660498395250301, 60.00099999999999767 ) ) ;
#12864 = CARTESIAN_POINT ( 'NONE',  ( 4.163799117100995136E-16, 9.999999999999998224, -3.399999999999995026 ) ) ;
#12865 = ORIENTED_EDGE ( 'NONE', *, *, #10725, .F. ) ;
#12866 = ADVANCED_FACE ( 'NONE', ( #11555 ), #21078, .F. ) ;
#12867 = CIRCLE ( 'NONE', #13221, 10.00000000000000355 ) ;
#12868 = ORIENTED_EDGE ( 'NONE', *, *, #3743, .T. ) ;
#12869 = VERTEX_POINT ( 'NONE', #902 ) ;
#12870 = ORIENTED_EDGE ( 'NONE', *, *, #6949, .T. ) ;
#12871 = CARTESIAN_POINT ( 'NONE',  ( 4.025500340002707844, -36.54278193890314697, -2.800654218530457484 ) ) ;
#12872 = DIRECTION ( 'NONE',  ( -1.296372316667914327E-16, -1.000000000000000000, 0.000000000000000000 ) ) ;
#12873 = CARTESIAN_POINT ( 'NONE',  ( 1.387778780781445676E-14, -1.000000000000028644, -48.73397172404115452 ) ) ;
#12874 = EDGE_LOOP ( 'NONE', ( #14599, #1573, #9975, #14647 ) ) ;
#12875 = DIRECTION ( 'NONE',  ( 6.505213034913038160E-19, 3.903127820947822896E-18, 1.000000000000000000 ) ) ;
#12876 = CARTESIAN_POINT ( 'NONE',  ( 1.387778780781445676E-14, 40.00000000000000000, 48.73397172404482802 ) ) ;
#12877 = VERTEX_POINT ( 'NONE', #2859 ) ;
#12878 = DIRECTION ( 'NONE',  ( 0.000000000000000000, -1.000000000000000000, 0.000000000000000000 ) ) ;
#12879 = CARTESIAN_POINT ( 'NONE',  ( 34.99999999999999289, -5.000000000000000000, -57.49999999999705835 ) ) ;
#12880 = CYLINDRICAL_SURFACE ( 'NONE', #12631, 60.00000000000000000 ) ;
#12881 = CARTESIAN_POINT ( 'NONE',  ( -35.00000000000000000, 25.00000000000000000, -8.999999999999989342 ) ) ;
#12882 = VECTOR ( 'NONE', #20607, 1000.000000000000000 ) ;
#12883 = VECTOR ( 'NONE', #7967, 1000.000000000000000 ) ;
#12884 = CARTESIAN_POINT ( 'NONE',  ( -20.00000000000001421, 20.00000000000000355, -105.0020000000000095 ) ) ;
#12885 = EDGE_CURVE ( 'NONE', #15727, #16891, #963, .T. ) ;
#12886 = DIRECTION ( 'NONE',  ( 0.000000000000000000, 0.000000000000000000, 1.000000000000000000 ) ) ;
#12887 = PRODUCT_DEFINITION ( 'UNKNOWN', '', #10935, #2800 ) ;
#12888 = FACE_OUTER_BOUND ( 'NONE', #367, .T. ) ;
#12889 = DIRECTION ( 'NONE',  ( 1.000000000000000000, 0.000000000000000000, 0.000000000000000000 ) ) ;
#12890 = ORIENTED_EDGE ( 'NONE', *, *, #6207, .F. ) ;
#12891 = VERTEX_POINT ( 'NONE', #2970 ) ;
#12892 = ORIENTED_EDGE ( 'NONE', *, *, #18740, .T. ) ;
#12893 = CIRCLE ( 'NONE', #4879, 19.11328065563152379 ) ;
#12894 = CARTESIAN_POINT ( 'NONE',  ( 2.775557561562891351E-14, -2.775557561562891351E-14, 2.999999999999999112 ) ) ;
#12895 = DIRECTION ( 'NONE',  ( 0.000000000000000000, 0.000000000000000000, -1.000000000000000000 ) ) ;
#12896 = CARTESIAN_POINT ( 'NONE',  ( -42.50000000000000711, -9.600000000000001421, -49.60000000000000142 ) ) ;
#12897 = AXIS2_PLACEMENT_3D ( 'NONE', #11154, #12634, #11040 ) ;
#12898 = EDGE_CURVE ( 'NONE', #21604, #6745, #13736, .T. ) ;
#12899 = CARTESIAN_POINT ( 'NONE',  ( 4.928914132345180823E-15, 7.999999999999994671, -19.00000000000000355 ) ) ;
#12900 = CARTESIAN_POINT ( 'NONE',  ( -8.619968867809234325, 38.06589896304013365, -54.65505050754611460 ) ) ;
#12901 = DIRECTION ( 'NONE',  ( -0.000000000000000000, -1.000000000000000000, -0.000000000000000000 ) ) ;
#12902 = CARTESIAN_POINT ( 'NONE',  ( -9.708269511265104512, 33.52953626616034200, -2.999999999999978240 ) ) ;
#12903 = ORIENTED_EDGE ( 'NONE', *, *, #9741, .T. ) ;
#12904 = CARTESIAN_POINT ( 'NONE',  ( 34.99999999999980815, 28.00000000000000000, 54.99999999999922551 ) ) ;
#12905 = DIRECTION ( 'NONE',  ( -1.000000000000000000, 0.000000000000000000, 0.000000000000000000 ) ) ;
#12906 = CARTESIAN_POINT ( 'NONE',  ( -14.93538271375420479, -34.13396246814581758, -2.999999999999999112 ) ) ;
#12907 = EDGE_CURVE ( 'NONE', #7488, #13097, #15575, .T. ) ;
#12908 = CYLINDRICAL_SURFACE ( 'NONE', #16960, 17.00000000000000000 ) ;
#12909 = ORIENTED_EDGE ( 'NONE', *, *, #18855, .F. ) ;
#12910 = CARTESIAN_POINT ( 'NONE',  ( 5.833333333333339255, 0.000000000000000000, 40.61164310337067462 ) ) ;
#12911 = CIRCLE ( 'NONE', #7431, 2.499999999999996891 ) ;
#12912 = FACE_OUTER_BOUND ( 'NONE', #19307, .T. ) ;
#12913 = CARTESIAN_POINT ( 'NONE',  ( 2.422192751864033156, 32.40961249803547872, -6.999999999999950262 ) ) ;
#12914 = DIRECTION ( 'NONE',  ( 6.505213034913038160E-19, 3.903127820947822896E-18, 1.000000000000000000 ) ) ;
#12915 = AXIS2_PLACEMENT_3D ( 'NONE', #18685, #18792, #6539 ) ;
#12916 = AXIS2_PLACEMENT_3D ( 'NONE', #14557, #17775, #9184 ) ;
#12917 = ORIENTED_EDGE ( 'NONE', *, *, #871, .F. ) ;
#12918 = DIRECTION ( 'NONE',  ( -6.505213034913038160E-19, -3.903127820947822896E-18, -1.000000000000000000 ) ) ;
#12919 = AXIS2_PLACEMENT_3D ( 'NONE', #21389, #4324, #2488 ) ;
#12920 = CARTESIAN_POINT ( 'NONE',  ( 2.734686107766180818, 40.00000000000000000, -50.39884022139948172 ) ) ;
#12921 = VERTEX_POINT ( 'NONE', #13363 ) ;
#12922 = CARTESIAN_POINT ( 'NONE',  ( 1.109394314766096068, 39.99267486917625547, -49.57771226710639212 ) ) ;
#12923 = DIRECTION ( 'NONE',  ( 6.505213034913038160E-19, 3.903127820947822896E-18, 1.000000000000000000 ) ) ;
#12924 = AXIS2_PLACEMENT_3D ( 'NONE', #18728, #9792, #10004 ) ;
#12925 = EDGE_CURVE ( 'NONE', #9204, #3967, #13004, .T. ) ;
#12926 = ORIENTED_EDGE ( 'NONE', *, *, #4433, .T. ) ;
#12927 = LINE ( 'NONE', #11343, #15083 ) ;
#12928 = CARTESIAN_POINT ( 'NONE',  ( -6.257499475795364141, 39.99999999999999289, 52.21447189357184726 ) ) ;
#12929 = ORIENTED_EDGE ( 'NONE', *, *, #21865, .T. ) ;
#12930 = CARTESIAN_POINT ( 'NONE',  ( -11.68090480754633553, 3.765577839755393619, -57.90797000640142045 ) ) ;
#12931 = CIRCLE ( 'NONE', #3076, 2.000000000000000444 ) ;
#12932 = CARTESIAN_POINT ( 'NONE',  ( -6.488130988471835892, 39.99999999999999289, 52.32258080686172264 ) ) ;
#12933 = DIRECTION ( 'NONE',  ( 1.000000000000000000, 1.208970125616063798E-17, 0.000000000000000000 ) ) ;
#12934 = ORIENTED_EDGE ( 'NONE', *, *, #3197, .F. ) ;
#12935 = DIRECTION ( 'NONE',  ( 0.000000000000000000, -1.000000000000000000, 0.000000000000000000 ) ) ;
#12936 = CARTESIAN_POINT ( 'NONE',  ( -11.68987541779232764, 3.735186999639990013, 55.40064774141873016 ) ) ;
#12937 = EDGE_CURVE ( 'NONE', #6950, #4080, #595, .T. ) ;
#12938 = EDGE_CURVE ( 'NONE', #14924, #15891, #8648, .T. ) ;
#12939 = CARTESIAN_POINT ( 'NONE',  ( 27.64365646977298852, 17.09029715894916279, -6.999999999999950262 ) ) ;
#12940 = ADVANCED_FACE ( 'NONE', ( #5247, #15315, #1233, #18769, #3418, #12225, #6738, #19226 ), #20719, .T. ) ;
#12941 = ORIENTED_EDGE ( 'NONE', *, *, #17816, .T. ) ;
#12942 = CARTESIAN_POINT ( 'NONE',  ( 1.110223024625156540E-13, -5.551115123125782702E-14, -6.999999999999950262 ) ) ;
#12943 = CARTESIAN_POINT ( 'NONE',  ( -48.93401015228426587, 10.00000000000000000, 46.57614213197968667 ) ) ;
#12944 = PRODUCT ( 'BOLT', 'BOLT', '', ( #19036 ) ) ;
#12945 = VECTOR ( 'NONE', #16489, 1000.000000000000000 ) ;
#12946 = EDGE_CURVE ( 'NONE', #14229, #2694, #8229, .T. ) ;
#12947 = PRESENTATION_LAYER_ASSIGNMENT (  '', '', ( #13668 ) ) ;
#12948 = ORIENTED_EDGE ( 'NONE', *, *, #8436, .T. ) ;
#12949 = ORIENTED_EDGE ( 'NONE', *, *, #6806, .T. ) ;
#12950 = ORIENTED_EDGE ( 'NONE', *, *, #12249, .T. ) ;
#12951 = CARTESIAN_POINT ( 'NONE',  ( 118.2725394482455101, 176.8704507353062354, 8.232483067896737339 ) ) ;
#12952 = VERTEX_POINT ( 'NONE', #4908 ) ;
#12953 = CARTESIAN_POINT ( 'NONE',  ( 15.27654436812519023, 32.91718622474422773, 59.27094897435730303 ) ) ;
#12954 = FACE_OUTER_BOUND ( 'NONE', #3359, .T. ) ;
#12955 = CARTESIAN_POINT ( 'NONE',  ( -23.65408649739124414, -22.22891329980541997, 3.000000000000023537 ) ) ;
#12956 = DIRECTION ( 'NONE',  ( 0.000000000000000000, 1.000000000000000000, 0.000000000000000000 ) ) ;
#12957 = EDGE_CURVE ( 'NONE', #15034, #18483, #14487, .T. ) ;
#12958 = AXIS2_PLACEMENT_3D ( 'NONE', #17811, #5897, #7614 ) ;
#12959 = FACE_OUTER_BOUND ( 'NONE', #5772, .T. ) ;
#12960 = ORIENTED_EDGE ( 'NONE', *, *, #7866, .F. ) ;
#12961 = DIRECTION ( 'NONE',  ( 1.296372316667914327E-16, 1.000000000000000000, -0.000000000000000000 ) ) ;
#12962 = CYLINDRICAL_SURFACE ( 'NONE', #17463, 0.9999999999999974465 ) ;
#12963 = ORIENTED_EDGE ( 'NONE', *, *, #18338, .F. ) ;
#12964 = DIRECTION ( 'NONE',  ( -1.000000000000000000, -1.208970125616077665E-17, 0.000000000000000000 ) ) ;
#12965 = CARTESIAN_POINT ( 'NONE',  ( -21.90353326617357510, 15.16496266307569130, -58.55331524747136029 ) ) ;
#12966 = DIRECTION ( 'NONE',  ( -0.000000000000000000, -1.000000000000000000, -0.000000000000000000 ) ) ;
#12967 = ORIENTED_EDGE ( 'NONE', *, *, #12557, .T. ) ;
#12968 = LINE ( 'NONE', #3644, #11940 ) ;
#12969 = CARTESIAN_POINT ( 'NONE',  ( 2.602085213965210642E-15, 0.000000000000000000, 0.000000000000000000 ) ) ;
#12970 = ORIENTED_EDGE ( 'NONE', *, *, #19112, .F. ) ;
#12971 = CARTESIAN_POINT ( 'NONE',  ( -42.50000000000000711, -5.000000000000000000, -49.60000000000000142 ) ) ;
#12972 = CARTESIAN_POINT ( 'NONE',  ( -9.103081159019568602, 0.03030367950605257835, -53.87333532811887693 ) ) ;
#12973 = ORIENTED_EDGE ( 'NONE', *, *, #13735, .F. ) ;
#12974 = CARTESIAN_POINT ( 'NONE',  ( -6.000000000000000000, 20.00000000000000000, -5.999999999999999112 ) ) ;
#12975 = CARTESIAN_POINT ( 'NONE',  ( 9.814839119318500948, 37.44644195123049002, 57.08682537453372419 ) ) ;
#12976 = CARTESIAN_POINT ( 'NONE',  ( 42.50000000000000711, -12.00000000000000000, 50.00000000000000711 ) ) ;
#12977 = CIRCLE ( 'NONE', #5676, 34.90673715956759082 ) ;
#12978 = EDGE_CURVE ( 'NONE', #11729, #12233, #17412, .T. ) ;
#12979 = EDGE_CURVE ( 'NONE', #10389, #15662, #3139, .T. ) ;
#12980 = CARTESIAN_POINT ( 'NONE',  ( -4.074925817841773323, 32.10132595304121850, -2.999999999999999112 ) ) ;
#12981 = EDGE_LOOP ( 'NONE', ( #10225, #112, #8752, #5519 ) ) ;
#12982 = ORIENTED_EDGE ( 'NONE', *, *, #13850, .T. ) ;
#12983 = ADVANCED_FACE ( 'NONE', ( #19007, #4799 ), #10275, .F. ) ;
#12984 = ORIENTED_EDGE ( 'NONE', *, *, #5767, .T. ) ;
#12985 = VERTEX_POINT ( 'NONE', #15423 ) ;
#12986 = CARTESIAN_POINT ( 'NONE',  ( 25.58633464742662866, 23.74488952252781715, 2.999999999999999112 ) ) ;
#12987 = CYLINDRICAL_SURFACE ( 'NONE', #8178, 2.500000000000008882 ) ;
#12988 = EDGE_LOOP ( 'NONE', ( #19710, #2550, #19262, #5989 ) ) ;
#12989 = FACE_OUTER_BOUND ( 'NONE', #9208, .T. ) ;
#12990 = DIRECTION ( 'NONE',  ( 0.1421319796954322312, 0.000000000000000000, -0.9898477157360405787 ) ) ;
#12991 = EDGE_LOOP ( 'NONE', ( #4868, #19259, #13577, #4840 ) ) ;
#12992 = CARTESIAN_POINT ( 'NONE',  ( -17.79229176513264932, -31.47226199422894410, -2.933296326616350758 ) ) ;
#12993 = SPHERICAL_SURFACE ( 'NONE', #11268, 41.25806096964027603 ) ;
#12994 = DIRECTION ( 'NONE',  ( 0.000000000000000000, 0.000000000000000000, -1.000000000000000000 ) ) ;
#12995 = DIRECTION ( 'NONE',  ( 0.000000000000000000, 1.000000000000000000, 0.000000000000000000 ) ) ;
#12996 = CIRCLE ( 'NONE', #8985, 36.76383501243555685 ) ;
#12997 = CARTESIAN_POINT ( 'NONE',  ( 24.73600648735135721, -27.19760187735867518, -2.000000000000005329 ) ) ;
#12998 = CARTESIAN_POINT ( 'NONE',  ( -1.387778780781445518E-14, 20.00000000000000355, -102.0000000000000142 ) ) ;
#12999 = DIRECTION ( 'NONE',  ( 1.296372316667914327E-16, 1.000000000000000000, -0.000000000000000000 ) ) ;
#13000 = AXIS2_PLACEMENT_3D ( 'NONE', #12390, #2196, #19398 ) ;
#13001 = ORIENTED_EDGE ( 'NONE', *, *, #3365, .F. ) ;
#13002 = ORIENTED_EDGE ( 'NONE', *, *, #904, .T. ) ;
#13003 = ORIENTED_EDGE ( 'NONE', *, *, #19534, .T. ) ;
#13004 = CIRCLE ( 'NONE', #11186, 6.499999999999999112 ) ;
#13005 = CYLINDRICAL_SURFACE ( 'NONE', #4551, 19.00000000000000355 ) ;
#13006 = CARTESIAN_POINT ( 'NONE',  ( -36.06598984771569860, 7.000000000000000000, -48.42385786802031333 ) ) ;
#13007 = EDGE_CURVE ( 'NONE', #10753, #9264, #15935, .T. ) ;
#13008 = DIRECTION ( 'NONE',  ( -6.505213034913038160E-19, -3.903127820947822896E-18, -1.000000000000000000 ) ) ;
#13009 = CARTESIAN_POINT ( 'NONE',  ( 1.575352350796998202, 39.94051438458651404, 50.55779643183549155 ) ) ;
#13010 = CARTESIAN_POINT ( 'NONE',  ( 32.27599279215780825, 14.85437171138566370, 3.000000000000047962 ) ) ;
#13011 = AXIS2_PLACEMENT_3D ( 'NONE', #20828, #10371, #17029 ) ;
#13012 = CARTESIAN_POINT ( 'NONE',  ( 5.816608766681834908, -4.770324936805408811, 49.23968220743229551 ) ) ;
#13013 = DIRECTION ( 'NONE',  ( -1.445602896647339163E-16, -0.000000000000000000, -1.000000000000000000 ) ) ;
#13014 = AXIS2_PLACEMENT_3D ( 'NONE', #19610, #17769, #22615 ) ;
#13015 = CARTESIAN_POINT ( 'NONE',  ( -16.66666666666666785, 20.00000000000000000, -23.57022603955158502 ) ) ;
#13016 = CIRCLE ( 'NONE', #7542, 58.99999999999702283 ) ;
#13017 = EDGE_CURVE ( 'NONE', #13636, #12273, #1470, .T. ) ;
#13018 = ORIENTED_EDGE ( 'NONE', *, *, #22202, .T. ) ;
#13019 = CARTESIAN_POINT ( 'NONE',  ( -25.00000000000000000, 20.00000000000000000, 6.487780019669002523E-15 ) ) ;
#13020 = DIRECTION ( 'NONE',  ( 0.000000000000000000, 1.000000000000000000, 0.000000000000000000 ) ) ;
#13021 = LINE ( 'NONE', #11326, #11943 ) ;
#13022 = DIRECTION ( 'NONE',  ( 6.505213034913038160E-19, 3.903127820947822896E-18, 1.000000000000000000 ) ) ;
#13023 = ORIENTED_EDGE ( 'NONE', *, *, #6746, .T. ) ;
#13024 = EDGE_LOOP ( 'NONE', ( #2299, #1092 ) ) ;
#13025 = DIRECTION ( 'NONE',  ( 0.000000000000000000, -0.000000000000000000, -1.000000000000000000 ) ) ;
#13026 = CARTESIAN_POINT ( 'NONE',  ( 33.52953626616048410, 9.708269511265299911, 2.999999999999995559 ) ) ;
#13027 = ORIENTED_EDGE ( 'NONE', *, *, #21574, .T. ) ;
#13028 = AXIS2_PLACEMENT_3D ( 'NONE', #1487, #5047, #18447 ) ;
#13029 = CARTESIAN_POINT ( 'NONE',  ( 2.220446049250313081E-13, -2.498001805406602216E-13, -6.859353255829918616 ) ) ;
#13030 = B_SPLINE_CURVE_WITH_KNOTS ( 'NONE', 1,
 ( #22117, #2981 ),
 .UNSPECIFIED., .F., .F.,
 ( 2, 2 ),
 ( 0.000000000000000000, 1.000000000000000000 ),
 .UNSPECIFIED. ) ;
#13031 = CARTESIAN_POINT ( 'NONE',  ( 6.445000816259396359, 40.00000000000000000, -52.30046220936269918 ) ) ;
#13032 = ADVANCED_FACE ( 'NONE', ( #17039 ), #10160, .F. ) ;
#13033 = EDGE_LOOP ( 'NONE', ( #9637, #6254, #21575, #5166 ) ) ;
#13034 = CARTESIAN_POINT ( 'NONE',  ( 4.517337970793025015, 39.87308997424864287, -51.91252392995636455 ) ) ;
#13035 = VECTOR ( 'NONE', #8392, 1000.000000000000000 ) ;
#13036 = CARTESIAN_POINT ( 'NONE',  ( 11.86180952233168995, 38.99999999999999289, 55.35904751184886408 ) ) ;
#13037 = DIRECTION ( 'NONE',  ( -0.000000000000000000, 1.000000000000000000, -0.000000000000000000 ) ) ;
#13038 = DIRECTION ( 'NONE',  ( 6.505213034913038160E-19, 3.903127820947822896E-18, 1.000000000000000000 ) ) ;
#13039 = CARTESIAN_POINT ( 'NONE',  ( 2.775557561562891351E-14, -2.775557561562891351E-14, 2.999999999999995559 ) ) ;
#13040 = FACE_OUTER_BOUND ( 'NONE', #16649, .T. ) ;
#13041 = EDGE_CURVE ( 'NONE', #15736, #10123, #22198, .T. ) ;
#13042 = CARTESIAN_POINT ( 'NONE',  ( 34.99999999999980815, 28.00000000000000000, 54.99999999999922551 ) ) ;
#13043 = VERTEX_POINT ( 'NONE', #6858 ) ;
#13044 = DIRECTION ( 'NONE',  ( -0.000000000000000000, -0.000000000000000000, 1.000000000000000000 ) ) ;
#13045 = AXIS2_PLACEMENT_3D ( 'NONE', #21556, #2186, #12379 ) ;
#13046 = DIRECTION ( 'NONE',  ( 6.505213034913038160E-19, 3.903127820947822896E-18, 1.000000000000000000 ) ) ;
#13047 = CYLINDRICAL_SURFACE ( 'NONE', #17323, 2.499999999999998668 ) ;
#13048 = CONICAL_SURFACE ( 'NONE', #9044, 2.525000000000110489, 0.7853981633971014453 ) ;
#13049 = ORIENTED_EDGE ( 'NONE', *, *, #13220, .F. ) ;
#13050 = CARTESIAN_POINT ( 'NONE',  ( 9.744263423230279386, 2.495070046657416718, 54.63687069583267686 ) ) ;
#13051 = CARTESIAN_POINT ( 'NONE',  ( -11.38359864655678244, 29.79463497853559417, 44.07478837098130953 ) ) ;
#13052 = DIRECTION ( 'NONE',  ( -6.505213034913038160E-19, -3.903127820947822896E-18, -1.000000000000000000 ) ) ;
#13053 = EDGE_CURVE ( 'NONE', #767, #4765, #18179, .T. ) ;
#13054 = ORIENTED_EDGE ( 'NONE', *, *, #7770, .F. ) ;
#13055 = VECTOR ( 'NONE', #2871, 1000.000000000000000 ) ;
#13056 = EDGE_LOOP ( 'NONE', ( #5364, #19195, #16316, #7073 ) ) ;
#13057 = DIRECTION ( 'NONE',  ( -0.9896250438806508676, 0.1436365362846999671, -0.003289068006899762038 ) ) ;
#13058 = EDGE_CURVE ( 'NONE', #3873, #4270, #10838, .T. ) ;
#13059 = ADVANCED_FACE ( 'NONE', ( #8680 ), #184, .T. ) ;
#13060 = AXIS2_PLACEMENT_3D ( 'NONE', #8688, #20953, #5257 ) ;
#13061 = ORIENTED_EDGE ( 'NONE', *, *, #2296, .T. ) ;
#13062 = CARTESIAN_POINT ( 'NONE',  ( 11.49399598612405349, 36.39311532300401097, 57.83624353974210663 ) ) ;
#13063 = CARTESIAN_POINT ( 'NONE',  ( 9.079900084790089920, 0.2952492082894785375, 53.92155889450688733 ) ) ;
#13064 = CARTESIAN_POINT ( 'NONE',  ( 31.92986134326233838, -18.22261011550282817, 2.800654218530512551 ) ) ;
#13065 = CARTESIAN_POINT ( 'NONE',  ( 17.86915608785671949, -27.01645732367871489, 3.000000000000002665 ) ) ;
#13066 = CARTESIAN_POINT ( 'NONE',  ( 28.49999999999998224, 19.99999999999999645, -105.0010000000000048 ) ) ;
#13067 = ORIENTED_EDGE ( 'NONE', *, *, #6955, .F. ) ;
#13068 = CARTESIAN_POINT ( 'NONE',  ( -14.85437171138578094, 32.27599279215743167, 3.000000000000051958 ) ) ;
#13069 = DIRECTION ( 'NONE',  ( 0.000000000000000000, 0.000000000000000000, 1.000000000000000000 ) ) ;
#13070 = EDGE_LOOP ( 'NONE', ( #21484, #3718, #7304, #13771 ) ) ;
#13071 = DIRECTION ( 'NONE',  ( -6.505213034913038160E-19, -3.903127820947822896E-18, -1.000000000000000000 ) ) ;
#13072 = DIRECTION ( 'NONE',  ( -1.000000000000000000, -1.208970125616077665E-17, 0.000000000000000000 ) ) ;
#13073 = CARTESIAN_POINT ( 'NONE',  ( 2.220446049250313081E-13, -8.326672684688674053E-14, 2.800654218530498785 ) ) ;
#13074 = ORIENTED_EDGE ( 'NONE', *, *, #17997, .F. ) ;
#13075 = CARTESIAN_POINT ( 'NONE',  ( 35.00000000000058265, 26.00000000000000355, -55.00000000000076028 ) ) ;
#13076 = DIRECTION ( 'NONE',  ( 0.000000000000000000, 0.000000000000000000, -1.000000000000000000 ) ) ;
#13077 = CIRCLE ( 'NONE', #2847, 19.99999999999999289 ) ;
#13078 = ORIENTED_EDGE ( 'NONE', *, *, #6945, .T. ) ;
#13079 = CARTESIAN_POINT ( 'NONE',  ( -1.609530493688067216E-14, 40.00000000000000000, 48.73397172404481381 ) ) ;
#13080 = EDGE_CURVE ( 'NONE', #14603, #4801, #19290, .T. ) ;
#13081 = CARTESIAN_POINT ( 'NONE',  ( -4.529250793106221700E-15, -0.2027636850925037537, -49.39727160457752575 ) ) ;
#13082 = ORIENTED_EDGE ( 'NONE', *, *, #14888, .T. ) ;
#13083 = CARTESIAN_POINT ( 'NONE',  ( 5.551115123125782702E-14, -1.387778780781445676E-13, -5.749999999999949374 ) ) ;
#13084 = CIRCLE ( 'NONE', #3597, 19.11328065563152379 ) ;
#13085 = AXIS2_PLACEMENT_3D ( 'NONE', #864, #4543, #4429 ) ;
#13086 = CARTESIAN_POINT ( 'NONE',  ( 90.00000000000000000, 40.00000000000000000, -2.500000000000003109 ) ) ;
#13087 = DIRECTION ( 'NONE',  ( 0.000000000000000000, 0.000000000000000000, -1.000000000000000000 ) ) ;
#13088 = CIRCLE ( 'NONE', #5439, 2.500000000000002220 ) ;
#13089 = CARTESIAN_POINT ( 'NONE',  ( 0.000000000000000000, 30.00000000000000000, 0.000000000000000000 ) ) ;
#13090 = CARTESIAN_POINT ( 'NONE',  ( 18.99835506942486418, 13.52193747355529219, -57.87905887291312723 ) ) ;
#13091 = EDGE_CURVE ( 'NONE', #19599, #22642, #8661, .T. ) ;
#13092 = VERTEX_POINT ( 'NONE', #7303 ) ;
#13093 = ORIENTED_EDGE ( 'NONE', *, *, #20991, .T. ) ;
#13094 = CIRCLE ( 'NONE', #6884, 28.00000000000000355 ) ;
#13095 = EDGE_LOOP ( 'NONE', ( #1950, #19384, #20677, #13832 ) ) ;
#13096 = ADVANCED_FACE ( 'NONE', ( #2147 ), #9015, .T. ) ;
#13097 = VERTEX_POINT ( 'NONE', #78 ) ;
#13098 = DIRECTION ( 'NONE',  ( -0.000000000000000000, -1.000000000000000000, -0.000000000000000000 ) ) ;
#13099 = AXIS2_PLACEMENT_3D ( 'NONE', #9906, #1093, #22060 ) ;
#13100 = DIRECTION ( 'NONE',  ( 0.000000000000000000, 0.000000000000000000, 1.000000000000000000 ) ) ;
#13101 = CONICAL_SURFACE ( 'NONE', #3253, 57.00000000000002132, 0.7853981633974437271 ) ;
#13102 = VECTOR ( 'NONE', #9070, 1000.000000000000000 ) ;
#13103 = VERTEX_POINT ( 'NONE', #9236 ) ;
#13104 = FACE_OUTER_BOUND ( 'NONE', #16285, .T. ) ;
#13105 = DIRECTION ( 'NONE',  ( 0.000000000000000000, -1.000000000000000000, 0.000000000000000000 ) ) ;
#13106 = ORIENTED_EDGE ( 'NONE', *, *, #2825, .F. ) ;
#13107 = CARTESIAN_POINT ( 'NONE',  ( 3.000000000000000888, 15.99999999999999645, 8.485281374238567764 ) ) ;
#13108 = ADVANCED_FACE ( 'NONE', ( #7066 ), #416, .F. ) ;
#13109 = ORIENTED_EDGE ( 'NONE', *, *, #12665, .F. ) ;
#13110 = CARTESIAN_POINT ( 'NONE',  ( 5.551115123125782702E-14, -1.387778780781445676E-13, -5.749999999999949374 ) ) ;
#13111 = ADVANCED_FACE ( 'NONE', ( #10956 ), #3906, .T. ) ;
#13112 = CARTESIAN_POINT ( 'NONE',  ( 18.22261011550282817, 31.92986134326228509, -1.999999999999977573 ) ) ;
#13113 = CARTESIAN_POINT ( 'NONE',  ( 3.053113317719180486E-13, -22.00000000000010303, -5.000000000000004441 ) ) ;
#13114 = CARTESIAN_POINT ( 'NONE',  ( -17.23507576850067835, 30.19164414353179637, -59.89185441256821463 ) ) ;
#13115 = AXIS2_PLACEMENT_3D ( 'NONE', #18651, #16815, #21317 ) ;
#13116 = EDGE_CURVE ( 'NONE', #7486, #1368, #9132, .T. ) ;
#13117 = AXIS2_PLACEMENT_3D ( 'NONE', #12048, #13742, #5072 ) ;
#13118 = CARTESIAN_POINT ( 'NONE',  ( -4.278324951949325161, 39.54020021135848140, 53.33400390260339918 ) ) ;
#13119 = DIRECTION ( 'NONE',  ( -1.000000000000000000, 0.000000000000000000, 0.000000000000000000 ) ) ;
#13120 = AXIS2_PLACEMENT_3D ( 'NONE', #16745, #5873, #5977 ) ;
#13121 = EDGE_LOOP ( 'NONE', ( #18006, #4525, #16422, #1851 ) ) ;
#13122 = VERTEX_POINT ( 'NONE', #3988 ) ;
#13123 = VERTEX_POINT ( 'NONE', #5573 ) ;
#13124 = CARTESIAN_POINT ( 'NONE',  ( -18.03138881840362373, 11.33611194795425448, 60.11697748794932039 ) ) ;
#13125 = DIRECTION ( 'NONE',  ( 0.000000000000000000, 0.000000000000000000, 1.000000000000000000 ) ) ;
#13126=STYLED_ITEM('',(#22727),#17721);
#13127 = CIRCLE ( 'NONE', #6561, 2.499999999999998668 ) ;
#13128 = CYLINDRICAL_SURFACE ( 'NONE', #8704, 0.9999999999999974465 ) ;
#13129 = CARTESIAN_POINT ( 'NONE',  ( 3.849727973822421485E-15, 1.499999999999994449, 0.000000000000000000 ) ) ;
#13130 = EDGE_CURVE ( 'NONE', #16148, #18333, #8306, .T. ) ;
#13131 = PLANE ( 'NONE',  #2431 ) ;
#13132 = DIRECTION ( 'NONE',  ( -1.000000000000000000, 1.686330027304618723E-14, 0.000000000000000000 ) ) ;
#13133 = CARTESIAN_POINT ( 'NONE',  ( -5.702716825708717074, 39.17357718829572377, -54.58701425223105019 ) ) ;
#13134 = PLANE ( 'NONE',  #7898 ) ;
#13135 = ORIENTED_EDGE ( 'NONE', *, *, #5495, .F. ) ;
#13136 = EDGE_CURVE ( 'NONE', #13854, #16362, #3867, .T. ) ;
#13137 = DIRECTION ( 'NONE',  ( 0.000000000000000000, 0.000000000000000000, -1.000000000000000000 ) ) ;
#13138 = CARTESIAN_POINT ( 'NONE',  ( -35.00000000000058265, 28.00000000000000000, -57.50000000000076028 ) ) ;
#13139 = CARTESIAN_POINT ( 'NONE',  ( 17.58064943503729083, 10.42262370234225166, 57.45835854660180786 ) ) ;
#13140 = DIRECTION ( 'NONE',  ( 6.505213034913038160E-19, 3.903127820947822896E-18, 1.000000000000000000 ) ) ;
#13141 = ORIENTED_EDGE ( 'NONE', *, *, #4723, .T. ) ;
#13142 = CARTESIAN_POINT ( 'NONE',  ( 3.330669073875469621E-13, -1.110223024625156540E-13, -2.999999999999971578 ) ) ;
#13143 = ORIENTED_EDGE ( 'NONE', *, *, #20991, .F. ) ;
#13144 = CIRCLE ( 'NONE', #20122, 2.499999999999996891 ) ;
#13145 = FACE_OUTER_BOUND ( 'NONE', #5600, .T. ) ;
#13146 = ORIENTED_EDGE ( 'NONE', *, *, #18317, .T. ) ;
#13147 = CARTESIAN_POINT ( 'NONE',  ( -34.99999999999980815, 28.00000000000000000, 52.89999999999922409 ) ) ;
#13148 = EDGE_CURVE ( 'NONE', #2570, #6570, #4268, .T. ) ;
#13149 = AXIS2_PLACEMENT_3D ( 'NONE', #10751, #12702, #342 ) ;
#13150 = CARTESIAN_POINT ( 'NONE',  ( 6.816855646551482018, 40.00000000000000711, -52.46799118524486971 ) ) ;
#13151 = VERTEX_POINT ( 'NONE', #10836 ) ;
#13152 = CARTESIAN_POINT ( 'NONE',  ( 1.095802490588493994, 39.99285411162865955, -49.56761786991830121 ) ) ;
#13153 = DIRECTION ( 'NONE',  ( 0.000000000000000000, 1.000000000000000000, 0.000000000000000000 ) ) ;
#13154 = ADVANCED_BREP_SHAPE_REPRESENTATION ( '', ( #17806, #18273 ), #5109 ) ;
#13155 = PRESENTATION_LAYER_ASSIGNMENT (  '', '', ( #2575 ) ) ;
#13156 = DIRECTION ( 'NONE',  ( -0.5002637533272162873, 0.000000000000000000, -0.8658730721687598608 ) ) ;
#13157 = CARTESIAN_POINT ( 'NONE',  ( -90.00000000000000000, 39.97500000000000142, -9.108981535246192915E-16 ) ) ;
#13158 = DIRECTION ( 'NONE',  ( -6.505213034913038160E-19, -3.903127820947822896E-18, -1.000000000000000000 ) ) ;
#13159 = CARTESIAN_POINT ( 'NONE',  ( -8.774779751595641386, 39.47272031439209883, 54.19450202971452768 ) ) ;
#13160 = CARTESIAN_POINT ( 'NONE',  ( 35.00000000000000000, 40.00000000000000000, -49.99999999999997868 ) ) ;
#13161 = ORIENTED_EDGE ( 'NONE', *, *, #6936, .T. ) ;
#13162 = DIRECTION ( 'NONE',  ( 0.000000000000000000, 0.000000000000000000, -1.000000000000000000 ) ) ;
#13163 = CARTESIAN_POINT ( 'NONE',  ( 90.00000000000000000, 40.00000000000000711, -2.525000000000000355 ) ) ;
#13164 = CARTESIAN_POINT ( 'NONE',  ( -0.02784959653163695745, 39.99999544702608745, -48.75564068409102703 ) ) ;
#13165 = EDGE_LOOP ( 'NONE', ( #3033, #12622, #5622, #5155 ) ) ;
#13166 = CARTESIAN_POINT ( 'NONE',  ( -15.00000000000001421, 20.00000000000000355, 45.82575694955841072 ) ) ;
#13167 = FACE_OUTER_BOUND ( 'NONE', #10860, .T. ) ;
#13168 = EDGE_CURVE ( 'NONE', #22583, #13103, #7185, .T. ) ;
#13169 = ORIENTED_EDGE ( 'NONE', *, *, #16776, .T. ) ;
#13170 = ADVANCED_FACE ( 'NONE', ( #21171 ), #532, .T. ) ;
#13171 = ORIENTED_EDGE ( 'NONE', *, *, #20274, .T. ) ;
#13172 = DIRECTION ( 'NONE',  ( -0.006752834798041749097, -0.9999753815462444351, -0.001906704915093601974 ) ) ;
#13173 = VERTEX_POINT ( 'NONE', #2024 ) ;
#13174 = CARTESIAN_POINT ( 'NONE',  ( 19.64447802513831220, 23.87744830687368136, 60.53680291695862792 ) ) ;
#13175 = DIRECTION ( 'NONE',  ( -0.000000000000000000, 1.000000000000000000, -0.000000000000000000 ) ) ;
#13176 = DIRECTION ( 'NONE',  ( 0.000000000000000000, 0.000000000000000000, 1.000000000000000000 ) ) ;
#13177 = CYLINDRICAL_SURFACE ( 'NONE', #13896, 2.500000000000002220 ) ;
#13178 = LINE ( 'NONE', #13066, #18237 ) ;
#13179 = VERTEX_POINT ( 'NONE', #21055 ) ;
#13180 = DIRECTION ( 'NONE',  ( 0.000000000000000000, 0.000000000000000000, 1.000000000000000000 ) ) ;
#13181 = DIRECTION ( 'NONE',  ( 1.000000000000000000, 0.000000000000000000, 0.000000000000000000 ) ) ;
#13182 = EDGE_LOOP ( 'NONE', ( #16514, #281, #19233, #3078, #10879 ) ) ;
#13183 = CARTESIAN_POINT ( 'NONE',  ( 2.220446049250313081E-13, -8.326672684688674053E-14, 2.800654218530498785 ) ) ;
#13184 = CARTESIAN_POINT ( 'NONE',  ( 7.088850870549147224E-15, -5.000000000000000000, 44.98888751680801334 ) ) ;
#13185 = CARTESIAN_POINT ( 'NONE',  ( 14.58570206007858694, 6.310259562106195652, -59.03202081059063033 ) ) ;
#13186 = ORIENTED_EDGE ( 'NONE', *, *, #3170, .T. ) ;
#13187 = DIRECTION ( 'NONE',  ( 0.000000000000000000, -1.000000000000000000, 0.000000000000000000 ) ) ;
#13188 = EDGE_CURVE ( 'NONE', #19486, #4044, #16108, .T. ) ;
#13189 = CARTESIAN_POINT ( 'NONE',  ( 7.538461658765248430, 38.52939893239186375, -55.92178727523597814 ) ) ;
#13190 = ORIENTED_EDGE ( 'NONE', *, *, #15353, .T. ) ;
#13191 = CARTESIAN_POINT ( 'NONE',  ( 6.297058390208000844, 38.99690150456885362, 53.73986305459201418 ) ) ;
#13192 = ORIENTED_EDGE ( 'NONE', *, *, #14888, .F. ) ;
#13193 = CARTESIAN_POINT ( 'NONE',  ( 13.88612301964874796, 34.41939562427457844, 58.78253654025287034 ) ) ;
#13194 = CARTESIAN_POINT ( 'NONE',  ( -18.00000000000001421, 20.00000000000000711, 105.0000000000000142 ) ) ;
#13195 = EDGE_CURVE ( 'NONE', #17781, #18716, #17500, .T. ) ;
#13196 = AXIS2_PLACEMENT_3D ( 'NONE', #17191, #7002, #17299 ) ;
#13197 = CARTESIAN_POINT ( 'NONE',  ( 16.72418712224170534, 8.992692292686992772, -57.18730031742025943 ) ) ;
#13198 = ORIENTED_EDGE ( 'NONE', *, *, #22362, .F. ) ;
#13199 = VERTEX_POINT ( 'NONE', #17610 ) ;
#13200 = ORIENTED_EDGE ( 'NONE', *, *, #16777, .T. ) ;
#13201 = ORIENTED_EDGE ( 'NONE', *, *, #2148, .F. ) ;
#13202 = CARTESIAN_POINT ( 'NONE',  ( 2.394928258270085930, 23.84763917262409549, 6.680059847312254995 ) ) ;
#13203 = CARTESIAN_POINT ( 'NONE',  ( -35.00000000000000000, 39.00000000000000711, 1.387778780781445676E-14 ) ) ;
#13204 = AXIS2_PLACEMENT_3D ( 'NONE', #21199, #9277, #7558 ) ;
#13205 = CIRCLE ( 'NONE', #2979, 2.525000000000110489 ) ;
#13206 = CARTESIAN_POINT ( 'NONE',  ( -7.463862311151203244, -35.99819890246958209, -2.000000000000001776 ) ) ;
#13207 = ORIENTED_EDGE ( 'NONE', *, *, #18168, .F. ) ;
#13208 = FACE_OUTER_BOUND ( 'NONE', #15613, .T. ) ;
#13209 = CARTESIAN_POINT ( 'NONE',  ( 2.979639132251328260, 15.60364968412344133, 6.492556366676851987 ) ) ;
#13210 = EDGE_LOOP ( 'NONE', ( #20068, #21936, #4438, #16299, #14438 ) ) ;
#13211 = CARTESIAN_POINT ( 'NONE',  ( 34.99999999999980815, 28.00000000000000000, 52.89999999999922409 ) ) ;
#13212 = EDGE_CURVE ( 'NONE', #3379, #13199, #15409, .T. ) ;
#13213 = ORIENTED_EDGE ( 'NONE', *, *, #3966, .T. ) ;
#13214 = DIRECTION ( 'NONE',  ( -1.000000000000000000, -1.208970125616046080E-17, 6.505213034913038160E-19 ) ) ;
#13215 = CARTESIAN_POINT ( 'NONE',  ( 34.88850421923997658, -1.128083539116281342, -2.999999999999971578 ) ) ;
#13216 = CARTESIAN_POINT ( 'NONE',  ( 3.330669073875469621E-13, -1.110223024625156540E-13, -2.999999999999971578 ) ) ;
#13217 = CARTESIAN_POINT ( 'NONE',  ( -19.43416121892457582, 24.82270088923175777, -60.48577746614100192 ) ) ;
#13218 = EDGE_CURVE ( 'NONE', #11241, #11580, #21475, .T. ) ;
#13219 = EDGE_CURVE ( 'NONE', #5859, #12070, #13762, .T. ) ;
#13220 = EDGE_CURVE ( 'NONE', #7098, #1277, #20242, .T. ) ;
#13221 = AXIS2_PLACEMENT_3D ( 'NONE', #6301, #22236, #16614 ) ;
#13222 = DIRECTION ( 'NONE',  ( -1.296372316667914327E-16, -1.000000000000000000, 0.000000000000000000 ) ) ;
#13223 = DIRECTION ( 'NONE',  ( 6.505213034913038160E-19, 3.903127820947822896E-18, 1.000000000000000000 ) ) ;
#13224 = VERTEX_POINT ( 'NONE', #18395 ) ;
#13225 = ORIENTED_EDGE ( 'NONE', *, *, #16086, .F. ) ;
#13226 = EDGE_CURVE ( 'NONE', #11834, #15811, #11204, .T. ) ;
#13227 = CARTESIAN_POINT ( 'NONE',  ( -17.19628968518555823, 9.778502620742683504, 59.87797704339187277 ) ) ;
#13228 = FACE_OUTER_BOUND ( 'NONE', #17220, .T. ) ;
#13229 = DIRECTION ( 'NONE',  ( -1.000000000000000000, 1.020425574104004369E-16, 0.000000000000000000 ) ) ;
#13230 = DIRECTION ( 'NONE',  ( 0.000000000000000000, 0.000000000000000000, -1.000000000000000000 ) ) ;
#13231 = CARTESIAN_POINT ( 'NONE',  ( 2.602085213965210642E-15, 6.000000000000019540, 0.000000000000000000 ) ) ;
#13232 = CYLINDRICAL_SURFACE ( 'NONE', #1790, 16.49999999999999645 ) ;
#13233 = CARTESIAN_POINT ( 'NONE',  ( -47.83731665821558465, 7.000000000000000000, 38.93845529828710283 ) ) ;
#13234 = CARTESIAN_POINT ( 'NONE',  ( -35.00000000000000000, 25.00000000000000000, -16.99999999999997868 ) ) ;
#13235 = CARTESIAN_POINT ( 'NONE',  ( -7.073806678778195689, 38.72385539215704142, -54.13592748070715288 ) ) ;
#13236 = ORIENTED_EDGE ( 'NONE', *, *, #8436, .F. ) ;
#13237 = DIRECTION ( 'NONE',  ( 0.000000000000000000, 0.7071067811865500152, 0.7071067811865451302 ) ) ;
#13238 = FACE_OUTER_BOUND ( 'NONE', #21099, .T. ) ;
#13239 = DIRECTION ( 'NONE',  ( 1.000000000000000000, 0.000000000000000000, 0.000000000000000000 ) ) ;
#13240 = ORIENTED_EDGE ( 'NONE', *, *, #359, .F. ) ;
#13241 = DIRECTION ( 'NONE',  ( 1.000000000000000000, 1.208970125616063028E-17, 0.000000000000000000 ) ) ;
#13242 = CARTESIAN_POINT ( 'NONE',  ( -5.816608766684079335, -4.770324936805427463, -49.23968220743358160 ) ) ;
#13243 = DIRECTION ( 'NONE',  ( 0.000000000000000000, -1.000000000000000000, 0.000000000000000000 ) ) ;
#13244 = EDGE_CURVE ( 'NONE', #9303, #8079, #16709, .T. ) ;
#13245 = TOROIDAL_SURFACE ( 'NONE', #21320, 34.90673715956759082, 8.750000000000000000 ) ;
#13246 = VECTOR ( 'NONE', #19067, 1000.000000000000114 ) ;
#13247 = EDGE_CURVE ( 'NONE', #57, #5656, #11410, .T. ) ;
#13248 = AXIS2_PLACEMENT_3D ( 'NONE', #13671, #20686, #4995 ) ;
#13249 = CARTESIAN_POINT ( 'NONE',  ( 0.6792558703086061245, -1.217297189599438445, 47.76386722475271540 ) ) ;
#13250 = EDGE_CURVE ( 'NONE', #5266, #16827, #5008, .T. ) ;
#13251 = DIRECTION ( 'NONE',  ( 0.000000000000000000, 0.000000000000000000, 1.000000000000000000 ) ) ;
#13252 = VERTEX_POINT ( 'NONE', #20132 ) ;
#13253 = CARTESIAN_POINT ( 'NONE',  ( 5.178711896350565169, 39.83381987255487644, -52.32443819789842365 ) ) ;
#13254 = CARTESIAN_POINT ( 'NONE',  ( 14.67611967928938910, -31.67162468656004037, 2.999999999999999112 ) ) ;
#13255 = CYLINDRICAL_SURFACE ( 'NONE', #17284, 3.999999999999996447 ) ;
#13256 = CARTESIAN_POINT ( 'NONE',  ( -90.00000000000000000, 40.00000000000000000, -9.108981535246192915E-16 ) ) ;
#13257 = DIRECTION ( 'NONE',  ( 0.000000000000000000, 0.000000000000000000, 1.000000000000000000 ) ) ;
#13258 = CARTESIAN_POINT ( 'NONE',  ( 42.50000000000000711, -5.000000000000000000, -45.40000000000000568 ) ) ;
#13259 = VECTOR ( 'NONE', #3517, 1000.000000000000000 ) ;
#13260 = CARTESIAN_POINT ( 'NONE',  ( 2.220446049250313081E-13, -2.498001805406602216E-13, -6.859353255829918616 ) ) ;
#13261 = ORIENTED_EDGE ( 'NONE', *, *, #9213, .F. ) ;
#13262 = LINE ( 'NONE', #13601, #15607 ) ;
#13263 = CARTESIAN_POINT ( 'NONE',  ( 2.422192751863949667, 32.40961249803550714, -2.999999999999995559 ) ) ;
#13264 =( GEOMETRIC_REPRESENTATION_CONTEXT ( 3 ) GLOBAL_UNCERTAINTY_ASSIGNED_CONTEXT ( ( #19960 ) ) GLOBAL_UNIT_ASSIGNED_CONTEXT ( ( #15026, #9988, #4515 ) ) REPRESENTATION_CONTEXT ( 'NONE', 'WORKASPACE' ) );
#13265 = CARTESIAN_POINT ( 'NONE',  ( 21.66577056626875475, -3.820259908672518634, -4.999999999999969802 ) ) ;
#13266 = CARTESIAN_POINT ( 'NONE',  ( -34.99999999999997868, -5.000000000000000000, 52.49999999999698730 ) ) ;
#13267 = VECTOR ( 'NONE', #1527, 1000.000000000000000 ) ;
#13268 = EDGE_LOOP ( 'NONE', ( #5922, #16936, #1199, #13078 ) ) ;
#13269 = CARTESIAN_POINT ( 'NONE',  ( -6.742883674876493316, -34.24928931925791176, -2.999999999999975131 ) ) ;
#13270 = DIRECTION ( 'NONE',  ( -1.000000000000000000, -1.208970125616057944E-17, 0.000000000000000000 ) ) ;
#13271 = ORIENTED_EDGE ( 'NONE', *, *, #6708, .F. ) ;
#13272 = CIRCLE ( 'NONE', #17321, 30.00000000000000000 ) ;
#13273 = VERTEX_POINT ( 'NONE', #2372 ) ;
#13274 = DIRECTION ( 'NONE',  ( 0.006752834798041697922, 0.9999753815462446571, 0.001906704915093594818 ) ) ;
#13275 = AXIS2_PLACEMENT_3D ( 'NONE', #16737, #8038, #13270 ) ;
#13276 = ORIENTED_EDGE ( 'NONE', *, *, #5673, .T. ) ;
#13277 = CARTESIAN_POINT ( 'NONE',  ( 15.58771758597473500, 32.56665981830160206, -59.37826087086040872 ) ) ;
#13278 = CARTESIAN_POINT ( 'NONE',  ( 42.50000000000000711, -12.00000000000012434, -47.50000000000000000 ) ) ;
#13279 = DIRECTION ( 'NONE',  ( 1.000000000000000000, 0.000000000000000000, 0.000000000000000000 ) ) ;
#13280 = DIRECTION ( 'NONE',  ( 6.505213034913038160E-19, 3.903127820947822896E-18, 1.000000000000000000 ) ) ;
#13281 = DIRECTION ( 'NONE',  ( -0.000000000000000000, -1.000000000000000000, -0.000000000000000000 ) ) ;
#13282 = EDGE_LOOP ( 'NONE', ( #18502, #13061 ) ) ;
#13283 = DIRECTION ( 'NONE',  ( 0.000000000000000000, -1.000000000000000000, 0.000000000000000000 ) ) ;
#13284 = DIRECTION ( 'NONE',  ( 0.7071067811865524577, 9.238438721427047137E-17, -0.7071067811865426878 ) ) ;
#13285 = ORIENTED_EDGE ( 'NONE', *, *, #18029, .F. ) ;
#13286 = CARTESIAN_POINT ( 'NONE',  ( -5.249999999999990230, 40.00000000000000000, -41.42387596543809991 ) ) ;
#13287 = EDGE_CURVE ( 'NONE', #22272, #22152, #2602, .T. ) ;
#13288 = DIRECTION ( 'NONE',  ( -6.505213034913038160E-19, -3.903127820947822896E-18, -1.000000000000000000 ) ) ;
#13289 = CARTESIAN_POINT ( 'NONE',  ( 25.00000000000000000, 20.00000000000000000, -24.99999999999999289 ) ) ;
#13290 = AXIS2_PLACEMENT_3D ( 'NONE', #3538, #3866, #1914 ) ;
#13291 = FACE_OUTER_BOUND ( 'NONE', #5575, .T. ) ;
#13292 = EDGE_LOOP ( 'NONE', ( #5, #13869, #15719, #15279 ) ) ;
#13293 = DIRECTION ( 'NONE',  ( -1.000000000000000000, 0.000000000000000000, 0.000000000000000000 ) ) ;
#13294 = CARTESIAN_POINT ( 'NONE',  ( 2.546709079545405707, 39.84786395731773467, -51.61893211308333917 ) ) ;
#13295 = ORIENTED_EDGE ( 'NONE', *, *, #7298, .F. ) ;
#13296 = DIRECTION ( 'NONE',  ( -1.000000000000000000, -1.208970125616063644E-17, 0.000000000000000000 ) ) ;
#13297 = CARTESIAN_POINT ( 'NONE',  ( 17.32050807568869644, -25.00000000000000000, 10.00000000000013323 ) ) ;
#13298 = EDGE_CURVE ( 'NONE', #11475, #18373, #18904, .T. ) ;
#13299 = ORIENTED_EDGE ( 'NONE', *, *, #13922, .F. ) ;
#13300 = LINE ( 'NONE', #4635, #3225 ) ;
#13301 = EDGE_CURVE ( 'NONE', #17574, #8936, #17437, .T. ) ;
#13302 = UNCERTAINTY_MEASURE_WITH_UNIT (LENGTH_MEASURE( 1.000000000000000082E-05 ), #598, 'distance_accuracy_value', 'NONE');
#13303 = AXIS2_PLACEMENT_3D ( 'NONE', #21063, #6976, #1583 ) ;
#13304 = CARTESIAN_POINT ( 'NONE',  ( 15.39832585462649028, 32.77960222724997408, 56.73873823673486783 ) ) ;
#13305 = CARTESIAN_POINT ( 'NONE',  ( -1.387778780781445518E-14, 20.00000000000000355, -102.0000000000000142 ) ) ;
#13306 = CIRCLE ( 'NONE', #2358, 31.50000000000001421 ) ;
#13307 = CARTESIAN_POINT ( 'NONE',  ( 15.06903587914752229, 33.17837898604023650, -59.20328215072071742 ) ) ;
#13308 = ORIENTED_EDGE ( 'NONE', *, *, #17223, .T. ) ;
#13309 = ORIENTED_EDGE ( 'NONE', *, *, #4115, .F. ) ;
#13310 = ADVANCED_FACE ( 'NONE', ( #14832 ), #989, .F. ) ;
#13311 = CIRCLE ( 'NONE', #5640, 36.76383501243555685 ) ;
#13312 = ORIENTED_EDGE ( 'NONE', *, *, #680, .T. ) ;
#13313 = ORIENTED_EDGE ( 'NONE', *, *, #11800, .F. ) ;
#13314 = DIRECTION ( 'NONE',  ( -0.000000000000000000, -1.000000000000000000, -0.000000000000000000 ) ) ;
#13315 = PRODUCT_DEFINITION_SHAPE ( 'NONE', 'NONE',  #22696 ) ;
#13316 = ORIENTED_EDGE ( 'NONE', *, *, #1012, .F. ) ;
#13317 = CARTESIAN_POINT ( 'NONE',  ( -28.14364593009900517, 21.69710536060289741, 3.000000000000042633 ) ) ;
#13318 = CARTESIAN_POINT ( 'NONE',  ( -2.916776610546922832, 15.20691911972858534, 6.515718972876874737 ) ) ;
#13319 = ORIENTED_EDGE ( 'NONE', *, *, #15606, .F. ) ;
#13320 = EDGE_CURVE ( 'NONE', #11887, #691, #14855, .T. ) ;
#13321 = LINE ( 'NONE', #18504, #9536 ) ;
#13322 = AXIS2_PLACEMENT_3D ( 'NONE', #9180, #12828, #19740 ) ;
#13323 = DIRECTION ( 'NONE',  ( 0.000000000000000000, 0.000000000000000000, -1.000000000000000000 ) ) ;
#13324 = ORIENTED_EDGE ( 'NONE', *, *, #9839, .F. ) ;
#13325 = DIRECTION ( 'NONE',  ( -1.000000000000000000, -1.208970125616081209E-17, 0.000000000000000000 ) ) ;
#13326 = CARTESIAN_POINT ( 'NONE',  ( -42.50000000000000711, -12.00000000000000000, -50.00000000000000000 ) ) ;
#13327 = CARTESIAN_POINT ( 'NONE',  ( -3.949642717238829380E-15, -1.890954608135210879, -47.89513957784965470 ) ) ;
#13328 = CARTESIAN_POINT ( 'NONE',  ( -19.85669122310597601, 22.43861522864551006, -60.58781117059879762 ) ) ;
#13329 = EDGE_CURVE ( 'NONE', #19408, #1795, #7927, .T. ) ;
#13330 = AXIS2_PLACEMENT_3D ( 'NONE', #16828, #5025, #12006 ) ;
#13331 = AXIS2_PLACEMENT_3D ( 'NONE', #1575, #17498, #1814 ) ;
#13332 = CYLINDRICAL_SURFACE ( 'NONE', #11886, 36.76383501243555685 ) ;
#13333 = ORIENTED_EDGE ( 'NONE', *, *, #11233, .F. ) ;
#13334 = ORIENTED_EDGE ( 'NONE', *, *, #22364, .T. ) ;
#13335 = EDGE_CURVE ( 'NONE', #9888, #16403, #12667, .T. ) ;
#13336 = AXIS2_PLACEMENT_3D ( 'NONE', #18829, #1637, #3131 ) ;
#13337 = VERTEX_POINT ( 'NONE', #19898 ) ;
#13338 = CARTESIAN_POINT ( 'NONE',  ( -18.69481036107322325, 7.531781294122753323, 57.74428367179859833 ) ) ;
#13339 = CARTESIAN_POINT ( 'NONE',  ( -35.00000000000000000, 17.00000000000000000, -38.99999999999999289 ) ) ;
#13340 = CIRCLE ( 'NONE', #6774, 2.499999999999998668 ) ;
#13341 = DIRECTION ( 'NONE',  ( -6.505213034913038160E-19, -3.903127820947822896E-18, -1.000000000000000000 ) ) ;
#13342 = FACE_OUTER_BOUND ( 'NONE', #17898, .T. ) ;
#13343 = EDGE_CURVE ( 'NONE', #4123, #18822, #4207, .T. ) ;
#13344 = VECTOR ( 'NONE', #6224, 1000.000000000000114 ) ;
#13345 = CYLINDRICAL_SURFACE ( 'NONE', #11563, 0.9999999999999991118 ) ;
#13346 = VERTEX_POINT ( 'NONE', #6034 ) ;
#13347 = LINE ( 'NONE', #1221, #11297 ) ;
#13348 = CARTESIAN_POINT ( 'NONE',  ( -35.00000000000058265, 40.00000000000000000, -57.10000000000076170 ) ) ;
#13349 = DIRECTION ( 'NONE',  ( 0.000000000000000000, 0.000000000000000000, -1.000000000000000000 ) ) ;
#13350 = CARTESIAN_POINT ( 'NONE',  ( 42.50000000000000000, 10.00000000000000000, 49.99999999999999289 ) ) ;
#13351 = DIRECTION ( 'NONE',  ( 0.000000000000000000, 0.000000000000000000, 1.000000000000000000 ) ) ;
#13352 = ORIENTED_EDGE ( 'NONE', *, *, #18151, .F. ) ;
#13353 = ADVANCED_FACE ( 'NONE', ( #7750 ), #14719, .F. ) ;
#13354 = LINE ( 'NONE', #12002, #19746 ) ;
#13355 = DIRECTION ( 'NONE',  ( 1.000000000000000000, -1.084202172485505420E-16, 0.000000000000000000 ) ) ;
#13356 = AXIS2_PLACEMENT_3D ( 'NONE', #2657, #4260, #4148 ) ;
#13357 = AXIS2_PLACEMENT_3D ( 'NONE', #3833, #10797, #17919 ) ;
#13358 = VERTEX_POINT ( 'NONE', #19521 ) ;
#13359 = DIRECTION ( 'NONE',  ( -1.000000000000000000, -1.208970125616077665E-17, 0.000000000000000000 ) ) ;
#13360 = CIRCLE ( 'NONE', #9718, 10.00000000000000000 ) ;
#13361 = DIRECTION ( 'NONE',  ( 0.000000000000000000, -1.000000000000000000, 0.000000000000000000 ) ) ;
#13362 = CARTESIAN_POINT ( 'NONE',  ( -34.99999999999997868, -5.000000000000000000, 54.99999999999698730 ) ) ;
#13363 = CARTESIAN_POINT ( 'NONE',  ( -7.524443153164889431, 20.67323765728973228, -2.999999999999978240 ) ) ;
#13364 = ADVANCED_FACE ( 'NONE', ( #10671 ), #4654, .F. ) ;
#13365 = TOROIDAL_SURFACE ( 'NONE', #17399, 34.90673715956759082, 8.750000000000000000 ) ;
#13366 = EDGE_LOOP ( 'NONE', ( #13917, #2911, #12853, #17073 ) ) ;
#13367 = AXIS2_PLACEMENT_3D ( 'NONE', #5137, #15650, #15414 ) ;
#13368 = EDGE_CURVE ( 'NONE', #4700, #15473, #14503, .T. ) ;
#13369 = ORIENTED_EDGE ( 'NONE', *, *, #8483, .T. ) ;
#13370 = DIRECTION ( 'NONE',  ( -0.000000000000000000, -1.000000000000000000, -0.000000000000000000 ) ) ;
#13371 = CARTESIAN_POINT ( 'NONE',  ( -42.50000000000000711, -3.738192700042122674, 47.50000000000000711 ) ) ;
#13372 = VECTOR ( 'NONE', #9574, 1000.000000000000000 ) ;
#13373 = ORIENTED_EDGE ( 'NONE', *, *, #8006, .F. ) ;
#13374 = AXIS2_PLACEMENT_3D ( 'NONE', #5328, #1887, #14118 ) ;
#13375 = LINE ( 'NONE', #11778, #17944 ) ;
#13376 = CARTESIAN_POINT ( 'NONE',  ( -24.73600648735095575, 27.19760187735845136, -2.800654218530457484 ) ) ;
#13377 = DIRECTION ( 'NONE',  ( -0.000000000000000000, 1.000000000000000000, -0.000000000000000000 ) ) ;
#13378 = CARTESIAN_POINT ( 'NONE',  ( -15.03694978696328732, 3.237610724667264961, -56.60357944353420123 ) ) ;
#13379 = EDGE_CURVE ( 'NONE', #454, #18218, #21588, .T. ) ;
#13380 = CARTESIAN_POINT ( 'NONE',  ( -13.07600923154788575, 27.35939529837144235, -44.93756990742565449 ) ) ;
#13381 = AXIS2_PLACEMENT_3D ( 'NONE', #6971, #15196, #17154 ) ;
#13382 = CARTESIAN_POINT ( 'NONE',  ( 35.00000000000001421, -5.000000000000000000, 1.540743955509788682E-30 ) ) ;
#13383 = VERTEX_POINT ( 'NONE', #11031 ) ;
#13384 = DIRECTION ( 'NONE',  ( 0.000000000000000000, -1.000000000000000000, 0.000000000000000000 ) ) ;
#13385 = FACE_BOUND ( 'NONE', #21964, .T. ) ;
#13386 = CARTESIAN_POINT ( 'NONE',  ( 9.062586715439639562, 2.130694986424134907, -54.31128890271873644 ) ) ;
#13387 = LINE ( 'NONE', #9747, #1215 ) ;
#13388 = EDGE_LOOP ( 'NONE', ( #20575, #20232, #13276 ) ) ;
#13389 = APPLICATION_CONTEXT ( 'automotive_design' ) ;
#13390 = CARTESIAN_POINT ( 'NONE',  ( -34.99999999999999289, -5.000000000000000000, 4.999999999999969802 ) ) ;
#13391 = CARTESIAN_POINT ( 'NONE',  ( -34.99999999999998579, -1.000000000000028644, -59.99999999999703704 ) ) ;
#13392 = CIRCLE ( 'NONE', #12662, 1.000000000000000888 ) ;
#13393 = VERTEX_POINT ( 'NONE', #12852 ) ;
#13394 = AXIS2_PLACEMENT_3D ( 'NONE', #12336, #7525, #5689 ) ;
#13395 = EDGE_LOOP ( 'NONE', ( #18820, #6592, #3382, #20452 ) ) ;
#13396 = ITEM_DEFINED_TRANSFORMATION ( 'NONE', 'NONE', #13120,  #18273 ) ;
#13397 = ORIENTED_EDGE ( 'NONE', *, *, #5114, .F. ) ;
#13398 = CARTESIAN_POINT ( 'NONE',  ( 19.29031483250422596, 25.30268833713984122, -60.44930483060156945 ) ) ;
#13399 = CARTESIAN_POINT ( 'NONE',  ( -42.50000000000000000, 7.000000000000000000, 47.49999999999999289 ) ) ;
#13400 = DIRECTION ( 'NONE',  ( -1.000000000000000000, -1.208970125616063644E-17, 0.000000000000000000 ) ) ;
#13401 = DIRECTION ( 'NONE',  ( 1.296372316667914327E-16, 1.000000000000000000, -0.000000000000000000 ) ) ;
#13402 = CARTESIAN_POINT ( 'NONE',  ( 2.855944605007590287, 5.272200938804487258, -39.14690304189951320 ) ) ;
#13403 = ORIENTED_EDGE ( 'NONE', *, *, #1866, .F. ) ;
#13404 = CYLINDRICAL_SURFACE ( 'NONE', #17529, 31.50000000000000711 ) ;
#13405 = DIRECTION ( 'NONE',  ( 1.000000000000000000, 2.269002777743560714E-17, 0.000000000000000000 ) ) ;
#13406 = ORIENTED_EDGE ( 'NONE', *, *, #10554, .T. ) ;
#13407 = DIRECTION ( 'NONE',  ( -1.000000000000000000, -1.208970125616063644E-17, 0.000000000000000000 ) ) ;
#13408 = EDGE_CURVE ( 'NONE', #4765, #8398, #16344, .T. ) ;
#13409 = CARTESIAN_POINT ( 'NONE',  ( 2.995584608082006106, -1.237002266245721627, -50.27666343020538164 ) ) ;
#13410 = DIRECTION ( 'NONE',  ( -1.000000000000000000, -2.677423277737400817E-15, 0.000000000000000000 ) ) ;
#13411 = CARTESIAN_POINT ( 'NONE',  ( 19.99999999999998579, 19.20373330966867442, -60.62177826491069510 ) ) ;
#13412 = EDGE_LOOP ( 'NONE', ( #8802, #4035, #12950, #6009, #5964, #20173, #15137 ) ) ;
#13413 = CARTESIAN_POINT ( 'NONE',  ( -3.995109296550547473, 40.00000000000000711, -51.09401224245644357 ) ) ;
#13414 = ORIENTED_EDGE ( 'NONE', *, *, #15318, .F. ) ;
#13415 = CARTESIAN_POINT ( 'NONE',  ( 2.775557561562891351E-14, -2.775557561562891351E-14, 2.999999999999999112 ) ) ;
#13416 = DIRECTION ( 'NONE',  ( 6.505213034913038160E-19, 3.903127820947822896E-18, 1.000000000000000000 ) ) ;
#13417 = EDGE_LOOP ( 'NONE', ( #21382, #9921, #19981, #4236 ) ) ;
#13418 = CARTESIAN_POINT ( 'NONE',  ( 30.98879172160187423, -17.38064605515599226, 3.000000000000061728 ) ) ;
#13419 = EDGE_CURVE ( 'NONE', #20633, #8824, #4293, .T. ) ;
#13420 = DIRECTION ( 'NONE',  ( -0.000000000000000000, -0.000000000000000000, -1.000000000000000000 ) ) ;
#13421 = DIRECTION ( 'NONE',  ( -1.000000000000000000, -1.208970125616060101E-17, 6.505213034913038160E-19 ) ) ;
#13422 = VECTOR ( 'NONE', #22031, 1000.000000000000000 ) ;
#13423 = CARTESIAN_POINT ( 'NONE',  ( 19.88905041091779324, 17.72428093567802776, -58.11830361001567979 ) ) ;
#13424 = CIRCLE ( 'NONE', #11616, 36.76383501243555685 ) ;
#13425 = AXIS2_PLACEMENT_3D ( 'NONE', #3333, #8700, #19130 ) ;
#13427 = VERTEX_POINT ( 'NONE', #8972 ) ;
#13426 = EDGE_CURVE ( 'NONE', #12156, #16900, #17801, .T. ) ;
#13428 = ORIENTED_EDGE ( 'NONE', *, *, #7897, .F. ) ;
#13429 = ORIENTED_EDGE ( 'NONE', *, *, #11396, .T. ) ;
#13430 = VERTEX_POINT ( 'NONE', #10916 ) ;
#13431 = CARTESIAN_POINT ( 'NONE',  ( -0.3890599827476972639, 25.00042110133432161, 7.000138250718057620 ) ) ;
#13432 = ADVANCED_FACE ( 'NONE', ( #7263 ), #18508, .F. ) ;
#13433 = AXIS2_PLACEMENT_3D ( 'NONE', #4961, #15138, #17209 ) ;
#13434 = CIRCLE ( 'NONE', #18212, 20.00000000000002132 ) ;
#13435 = ORIENTED_EDGE ( 'NONE', *, *, #21288, .F. ) ;
#13436 = LINE ( 'NONE', #9797, #11639 ) ;
#13437 = CARTESIAN_POINT ( 'NONE',  ( -5.079212789376158277, -3.097595057465493795, -50.74825967503716839 ) ) ;
#13438 = EDGE_LOOP ( 'NONE', ( #6802, #20190, #15718, #14963 ) ) ;
#13439 = CARTESIAN_POINT ( 'NONE',  ( 11.93972437435558653, 29.14949368109859407, -7.000000000000006217 ) ) ;
#13440 = CIRCLE ( 'NONE', #21150, 0.9999999999999974465 ) ;
#13441 = ORIENTED_EDGE ( 'NONE', *, *, #12688, .T. ) ;
#13442 = CARTESIAN_POINT ( 'NONE',  ( 5.702716825709497783, 39.17357718829546798, -54.58701425223458870 ) ) ;
#13443 = CIRCLE ( 'NONE', #4690, 18.00000000000000000 ) ;
#13444 = DIRECTION ( 'NONE',  ( -1.000000000000000000, 0.000000000000000000, 0.000000000000000000 ) ) ;
#13445 = CARTESIAN_POINT ( 'NONE',  ( 12.99999999999993960, 42.51666049839543149, 105.0000000000000142 ) ) ;
#13446 = AXIS2_PLACEMENT_3D ( 'NONE', #17386, #16114, #3427 ) ;
#13447 = CARTESIAN_POINT ( 'NONE',  ( -9.940687323067972869, 37.37897894777885455, -57.14641600008366851 ) ) ;
#13448 = CARTESIAN_POINT ( 'NONE',  ( -14.52224280010138280, 16.16745304956414486, 45.61498238574518638 ) ) ;
#13449 = ORIENTED_EDGE ( 'NONE', *, *, #16157, .F. ) ;
#13450 = CIRCLE ( 'NONE', #16026, 22.12933039895921539 ) ;
#13451 = CIRCLE ( 'NONE', #20813, 25.00000000000000711 ) ;
#13452 = ORIENTED_EDGE ( 'NONE', *, *, #13368, .F. ) ;
#13453 = CIRCLE ( 'NONE', #6527, 2.499999999999995115 ) ;
#13454 = VECTOR ( 'NONE', #15462, 1000.000000000000114 ) ;
#13455 = ORIENTED_EDGE ( 'NONE', *, *, #16143, .T. ) ;
#13456 = CARTESIAN_POINT ( 'NONE',  ( -14.69246073108895168, 6.394048232430655787, 56.48929660089485338 ) ) ;
#13457 = EDGE_CURVE ( 'NONE', #17863, #15580, #5534, .T. ) ;
#13458 = LINE ( 'NONE', #11755, #2689 ) ;
#13459 = DIRECTION ( 'NONE',  ( 0.000000000000000000, 0.000000000000000000, 1.000000000000000000 ) ) ;
#13460 = DIRECTION ( 'NONE',  ( 1.000000000000000000, 0.000000000000000000, 0.000000000000000000 ) ) ;
#13461 = CARTESIAN_POINT ( 'NONE',  ( -30.33632613426173918, 11.35354668330684724, -6.999999999999957367 ) ) ;
#13462 = CIRCLE ( 'NONE', #315, 3.000000000000002665 ) ;
#13463 = ORIENTED_EDGE ( 'NONE', *, *, #21253, .F. ) ;
#13464 = CARTESIAN_POINT ( 'NONE',  ( 0.000000000000000000, 7.000000000000000000, 0.000000000000000000 ) ) ;
#13465 = CARTESIAN_POINT ( 'NONE',  ( -5.345263555475219697, 39.99999999999999289, -51.78208643630931363 ) ) ;
#13466 = AXIS2_PLACEMENT_3D ( 'NONE', #12154, #3463, #5290 ) ;
#13467 = CARTESIAN_POINT ( 'NONE',  ( -34.13396246814566837, 14.93538271375394189, -6.999999999999985789 ) ) ;
#13468 = CARTESIAN_POINT ( 'NONE',  ( 31.88709182564697286, -6.070730550690988991, -2.999999999999971578 ) ) ;
#13469 = AXIS2_PLACEMENT_3D ( 'NONE', #18210, #12918, #2639 ) ;
#13470 = EDGE_CURVE ( 'NONE', #7904, #8190, #9779, .T. ) ;
#13471 = VERTEX_POINT ( 'NONE', #21466 ) ;
#13472 = CARTESIAN_POINT ( 'NONE',  ( -10.78076590482871211, 39.17366535989417287, 54.93576791444288432 ) ) ;
#13473 = CARTESIAN_POINT ( 'NONE',  ( 1.110223024625156540E-13, -5.551115123125782702E-14, -6.999999999999950262 ) ) ;
#13474 = CIRCLE ( 'NONE', #18985, 17.00000000000000711 ) ;
#13475 = VERTEX_POINT ( 'NONE', #12508 ) ;
#13476 = DIRECTION ( 'NONE',  ( 0.000000000000000000, 1.000000000000000000, 0.000000000000000000 ) ) ;
#13477 = CYLINDRICAL_SURFACE ( 'NONE', #3102, 50.00000000000000000 ) ;
#13478 = DIRECTION ( 'NONE',  ( -0.000000000000000000, 1.000000000000000000, -0.000000000000000000 ) ) ;
#13479 = ADVANCED_FACE ( 'NONE', ( #15955 ), #19758, .F. ) ;
#13480 = ORIENTED_EDGE ( 'NONE', *, *, #3649, .F. ) ;
#13481 = AXIS2_PLACEMENT_3D ( 'NONE', #300, #5915, #9127 ) ;
#13482 = CIRCLE ( 'NONE', #8387, 2.500000000000002220 ) ;
#13483 = ORIENTED_EDGE ( 'NONE', *, *, #7385, .T. ) ;
#13484 = LINE ( 'NONE', #22111, #1609 ) ;
#13485 = DIRECTION ( 'NONE',  ( -6.505213034913038160E-19, -3.903127820947822896E-18, -1.000000000000000000 ) ) ;
#13486 = ORIENTED_EDGE ( 'NONE', *, *, #12137, .F. ) ;
#13487 = DIRECTION ( 'NONE',  ( 0.5002637533272700221, 0.000000000000000000, -0.8658730721687286636 ) ) ;
#13488 = CARTESIAN_POINT ( 'NONE',  ( 35.00000000000058265, 28.00000000000000000, -57.10000000000076170 ) ) ;
#13489 = CARTESIAN_POINT ( 'NONE',  ( -2.425350241063221279, 40.00000000000000000, 50.22136039941155161 ) ) ;
#13490 = CARTESIAN_POINT ( 'NONE',  ( -21.22368364729210910, 12.66551901741667585, -58.39771426751148198 ) ) ;
#13491 = CARTESIAN_POINT ( 'NONE',  ( -7.259789697909740269, 39.65417261969281526, 53.48039063277445848 ) ) ;
#13492 = CARTESIAN_POINT ( 'NONE',  ( -17.17026400045400436, 34.49621688465821023, 57.29349885535140174 ) ) ;
#13493 = ADVANCED_FACE ( 'NONE', ( #17573 ), #17914, .F. ) ;
#13494 = AXIS2_PLACEMENT_3D ( 'NONE', #6825, #21027, #5116 ) ;
#13495 = ORIENTED_EDGE ( 'NONE', *, *, #15621, .F. ) ;
#13496 = CARTESIAN_POINT ( 'NONE',  ( 7.711478842616803497, -31.57187188083537777, -7.000000000000006217 ) ) ;
#13497 = LINE ( 'NONE', #7918, #6373 ) ;
#13498 = DIRECTION ( 'NONE',  ( 6.505213034913038160E-19, 3.903127820947822896E-18, 1.000000000000000000 ) ) ;
#13499 = DIRECTION ( 'NONE',  ( 0.000000000000000000, 0.000000000000000000, 1.000000000000000000 ) ) ;
#13500 = ORIENTED_EDGE ( 'NONE', *, *, #2081, .F. ) ;
#13501 = CARTESIAN_POINT ( 'NONE',  ( -13.56354382738803466, 2.142135623730931471, 56.03997097393687454 ) ) ;
#13502 = DIRECTION ( 'NONE',  ( 0.000000000000000000, 0.000000000000000000, 1.000000000000000000 ) ) ;
#13503 = DIRECTION ( 'NONE',  ( -6.505213034913038160E-19, -3.903127820947822896E-18, -1.000000000000000000 ) ) ;
#13504 = EDGE_CURVE ( 'NONE', #10205, #14672, #6059, .T. ) ;
#13505 = EDGE_CURVE ( 'NONE', #43, #9799, #17327, .T. ) ;
#13506 = EDGE_CURVE ( 'NONE', #13935, #21335, #9201, .T. ) ;
#13507 = SHAPE_REPRESENTATION ( 'FRONT COVER', ( #18273 ), #22681 ) ;
#13508 = ORIENTED_EDGE ( 'NONE', *, *, #10471, .T. ) ;
#13509 = VECTOR ( 'NONE', #20014, 1000.000000000000000 ) ;
#13510 = EDGE_CURVE ( 'NONE', #17179, #11978, #488, .T. ) ;
#13511 = ORIENTED_EDGE ( 'NONE', *, *, #18574, .F. ) ;
#13512 = PRODUCT_CONTEXT ( 'NONE', #14261, 'mechanical' ) ;
#13513 = ORIENTED_EDGE ( 'NONE', *, *, #590, .F. ) ;
#13514 = CARTESIAN_POINT ( 'NONE',  ( -21.41958700883257904, -27.56232195404059837, -2.999999999999992450 ) ) ;
#13515 = CARTESIAN_POINT ( 'NONE',  ( -2.999999999999999112, 16.00000000000000000, 8.485281374238567764 ) ) ;
#13516 = DIRECTION ( 'NONE',  ( -6.505213034913038160E-19, -3.903127820947822896E-18, -1.000000000000000000 ) ) ;
#13517 = CARTESIAN_POINT ( 'NONE',  ( 21.99999999999998579, 20.00000000000000355, -100.0000000000000000 ) ) ;
#13518 = DIRECTION ( 'NONE',  ( -1.000000000000000000, 0.000000000000000000, 0.000000000000000000 ) ) ;
#13519 = VERTEX_POINT ( 'NONE', #5769 ) ;
#13520 = CYLINDRICAL_SURFACE ( 'NONE', #3628, 19.11328065563150957 ) ;
#13521 = DIRECTION ( 'NONE',  ( 0.000000000000000000, -1.000000000000000000, 0.000000000000000000 ) ) ;
#13522 = ORIENTED_EDGE ( 'NONE', *, *, #6770, .T. ) ;
#13523 = DIRECTION ( 'NONE',  ( 1.000000000000000000, 0.000000000000000000, 0.000000000000000000 ) ) ;
#13524 = CARTESIAN_POINT ( 'NONE',  ( 28.07080038625115037, 14.29266125237890783, -6.999999999999950262 ) ) ;
#13526 = AXIS2_PLACEMENT_3D ( 'NONE', #4365, #1027, #14868 ) ;
#13525 = CARTESIAN_POINT ( 'NONE',  ( -35.00000000000000000, 0.000000000000000000, 2.365113165210053967E-14 ) ) ;
#13527 = CARTESIAN_POINT ( 'NONE',  ( 9.455104429560558188, 39.37252125300741312, 54.46735621542109840 ) ) ;
#13528 = VERTEX_POINT ( 'NONE', #4063 ) ;
#13529 = DIRECTION ( 'NONE',  ( 0.000000000000000000, 0.000000000000000000, -1.000000000000000000 ) ) ;
#13530 = ORIENTED_EDGE ( 'NONE', *, *, #7207, .T. ) ;
#13531 = PLANE ( 'NONE',  #220 ) ;
#13532 = CARTESIAN_POINT ( 'NONE',  ( -14.68518659845081409, 36.96998281527654484, 56.45735093204006461 ) ) ;
#13533 = ORIENTED_EDGE ( 'NONE', *, *, #18889, .T. ) ;
#13534 = DIRECTION ( 'NONE',  ( -1.000000000000000000, 0.000000000000000000, 0.000000000000000000 ) ) ;
#13535 = CARTESIAN_POINT ( 'NONE',  ( 3.330669073875469621E-13, -1.110223024625156540E-13, -2.999999999999971578 ) ) ;
#13536 = DIRECTION ( 'NONE',  ( 0.000000000000000000, 1.000000000000000000, -0.000000000000000000 ) ) ;
#13537 = CARTESIAN_POINT ( 'NONE',  ( 18.85220035178958042, 32.22744690108880405, -57.78902400853694843 ) ) ;
#13539 = EDGE_CURVE ( 'NONE', #131, #2473, #14131, .T. ) ;
#13538 = ORIENTED_EDGE ( 'NONE', *, *, #12170, .T. ) ;
#13540 = AXIS2_PLACEMENT_3D ( 'NONE', #8238, #19123, #8691 ) ;
#13541 = ADVANCED_FACE ( 'NONE', ( #21932 ), #11143, .T. ) ;
#13542 = VERTEX_POINT ( 'NONE', #18137 ) ;
#13543 = ORIENTED_EDGE ( 'NONE', *, *, #6074, .T. ) ;
#13544 =( NAMED_UNIT ( * ) PLANE_ANGLE_UNIT ( ) SI_UNIT ( $, .RADIAN. ) );
#13545 = VERTEX_POINT ( 'NONE', #4509 ) ;
#13546 = CARTESIAN_POINT ( 'NONE',  ( -0.7842774244934771488, 24.91897157216331848, 6.973256348169272201 ) ) ;
#13547 = DIRECTION ( 'NONE',  ( -0.000000000000000000, -0.000000000000000000, 1.000000000000000000 ) ) ;
#13548 = EDGE_CURVE ( 'NONE', #13199, #10901, #14867, .T. ) ;
#13549 = ORIENTED_EDGE ( 'NONE', *, *, #9723, .F. ) ;
#13550 = CARTESIAN_POINT ( 'NONE',  ( 31.41239365194237365, -2.347663744114464102, 3.000000000000023537 ) ) ;
#13551 = CARTESIAN_POINT ( 'NONE',  ( -9.079900084793857573, 0.2952492082908969584, -53.92155889450898343 ) ) ;
#13552 = ORIENTED_EDGE ( 'NONE', *, *, #5485, .F. ) ;
#13553 = CARTESIAN_POINT ( 'NONE',  ( -3.000000000000000000, 15.20121272115292044, 6.485281374238567764 ) ) ;
#13554 = ORIENTED_EDGE ( 'NONE', *, *, #22211, .T. ) ;
#13555 = FACE_OUTER_BOUND ( 'NONE', #12817, .T. ) ;
#13556 = VECTOR ( 'NONE', #3612, 1000.000000000000000 ) ;
#13557 = CARTESIAN_POINT ( 'NONE',  ( -13.74639653023206520, 28.96193690644924246, -2.999999999999968026 ) ) ;
#13558 = CARTESIAN_POINT ( 'NONE',  ( -36.75746821813305587, 0.6841746959067307454, 2.800654218530485018 ) ) ;
#13559 = CARTESIAN_POINT ( 'NONE',  ( -0.3011557478976217284, 39.99946772338066836, 48.96697170734454829 ) ) ;
#13560 = AXIS2_PLACEMENT_3D ( 'NONE', #21122, #601, #14567 ) ;
#13561 = EDGE_CURVE ( 'NONE', #20205, #3398, #12679, .T. ) ;
#13562 = DIRECTION ( 'NONE',  ( 0.000000000000000000, 0.000000000000000000, -1.000000000000000000 ) ) ;
#13563 = VERTEX_POINT ( 'NONE', #1072 ) ;
#13564 = CONICAL_SURFACE ( 'NONE', #19453, 2.099999999999997868, 1.029744258676653867 ) ;
#13565 = ORIENTED_EDGE ( 'NONE', *, *, #9847, .F. ) ;
#13566 = ORIENTED_EDGE ( 'NONE', *, *, #2839, .F. ) ;
#13567 = ORIENTED_EDGE ( 'NONE', *, *, #14974, .T. ) ;
#13568 = CARTESIAN_POINT ( 'NONE',  ( -17.29817675749697514, 30.08054145047330508, 57.37022932959109056 ) ) ;
#13569 = CARTESIAN_POINT ( 'NONE',  ( 26.50842683089782525, -24.41514043009201984, -6.999999999999992006 ) ) ;
#13570 = FACE_OUTER_BOUND ( 'NONE', #5745, .T. ) ;
#13571 = CARTESIAN_POINT ( 'NONE',  ( -11.59091061707577275, 39.99999999999998579, 54.17810196248734655 ) ) ;
#13572 = ORIENTED_EDGE ( 'NONE', *, *, #10940, .T. ) ;
#13573 = LINE ( 'NONE', #11873, #7277 ) ;
#13574 = CARTESIAN_POINT ( 'NONE',  ( -8.616492346064047680, 40.00000000000000000, -53.19943576996322321 ) ) ;
#13575 = DIRECTION ( 'NONE',  ( -6.505213034913038160E-19, -3.903127820947822896E-18, -1.000000000000000000 ) ) ;
#13576 = EDGE_CURVE ( 'NONE', #1383, #16162, #1171, .T. ) ;
#13577 = ORIENTED_EDGE ( 'NONE', *, *, #13947, .T. ) ;
#13578 = DIRECTION ( 'NONE',  ( -0.000000000000000000, -0.000000000000000000, -1.000000000000000000 ) ) ;
#13579 = EDGE_CURVE ( 'NONE', #6038, #3138, #6657, .T. ) ;
#13580 = EDGE_LOOP ( 'NONE', ( #6811, #20221, #11505, #8950 ) ) ;
#13581 = EDGE_CURVE ( 'NONE', #6508, #18887, #3389, .T. ) ;
#13582 = DIRECTION ( 'NONE',  ( -1.000000000000000000, 0.000000000000000000, 0.000000000000000000 ) ) ;
#13583 = LINE ( 'NONE', #4577, #15885 ) ;
#13584 = DIRECTION ( 'NONE',  ( 1.000000000000000000, -1.296372316667914327E-16, 0.000000000000000000 ) ) ;
#13585 = ORIENTED_EDGE ( 'NONE', *, *, #11777, .F. ) ;
#13586 = EDGE_LOOP ( 'NONE', ( #21156, #2349, #9533, #20694, #7506, #22126 ) ) ;
#13587 = CARTESIAN_POINT ( 'NONE',  ( -0.2357944722115355995, -1.232758281750954144, 48.43260639659581557 ) ) ;
#13588 = CIRCLE ( 'NONE', #11044, 19.11328065563151668 ) ;
#13589 = EDGE_CURVE ( 'NONE', #17185, #4605, #20021, .T. ) ;
#13590 = CARTESIAN_POINT ( 'NONE',  ( -21.65063509461084834, 12.49999999999967848, -2.999999999999988898 ) ) ;
#13591 = ORIENTED_EDGE ( 'NONE', *, *, #21032, .F. ) ;
#13592 = CARTESIAN_POINT ( 'NONE',  ( 19.99999999999998579, 20.00000000000000000, 98.00000000000000000 ) ) ;
#13593 = B_SPLINE_CURVE_WITH_KNOTS ( 'NONE', 3,
 ( #9317, #12504, #11026, #2322 ),
 .UNSPECIFIED., .F., .F.,
 ( 4, 4 ),
 ( 9.545285768313558837E-07, 0.001900595205834684732 ),
 .UNSPECIFIED. ) ;
#13594 = CARTESIAN_POINT ( 'NONE',  ( 6.000000000000000888, 0.000000000000000000, 6.000000000000000000 ) ) ;
#13595 = CARTESIAN_POINT ( 'NONE',  ( 90.00000000000000000, 28.00000000000000000, -9.108981535246192915E-16 ) ) ;
#13596 = EDGE_CURVE ( 'NONE', #31, #16039, #8166, .T. ) ;
#13597 = CARTESIAN_POINT ( 'NONE',  ( -22.38794582965170221, 21.29119307984318255, -58.65949541090341057 ) ) ;
#13598 = CARTESIAN_POINT ( 'NONE',  ( -7.899720326450768049, 39.58366711203084520, 53.79762300408461329 ) ) ;
#13599 = CARTESIAN_POINT ( 'NONE',  ( -15.21899206303018026, 36.51951236530621969, 56.65045400726779690 ) ) ;
#13600 = ORIENTED_EDGE ( 'NONE', *, *, #18581, .F. ) ;
#13601 = CARTESIAN_POINT ( 'NONE',  ( 25.00000000000000355, 20.00000000000000000, 25.00000000000000711 ) ) ;
#13602 = FACE_BOUND ( 'NONE', #19074, .T. ) ;
#13603 = DIRECTION ( 'NONE',  ( -0.000000000000000000, -0.000000000000000000, -1.000000000000000000 ) ) ;
#13604 = CARTESIAN_POINT ( 'NONE',  ( -26.00000000000001421, 19.99999999999982947, 60.00099999999999767 ) ) ;
#13605 = ORIENTED_EDGE ( 'NONE', *, *, #1318, .T. ) ;
#13606 = AXIS2_PLACEMENT_3D ( 'NONE', #9791, #13314, #20224 ) ;
#13607 = DIRECTION ( 'NONE',  ( 1.000000000000000000, 0.000000000000000000, 0.000000000000000000 ) ) ;
#13608 = CYLINDRICAL_SURFACE ( 'NONE', #10019, 19.11328065563152379 ) ;
#13609 = CARTESIAN_POINT ( 'NONE',  ( 1.102182119232617517E-15, 30.00000000000000000, 8.999999999999998224 ) ) ;
#13610 = VECTOR ( 'NONE', #6944, 1000.000000000000000 ) ;
#13611 = ORIENTED_EDGE ( 'NONE', *, *, #12656, .T. ) ;
#13612 = EDGE_CURVE ( 'NONE', #105, #15831, #13781, .T. ) ;
#13613 = ORIENTED_EDGE ( 'NONE', *, *, #8890, .T. ) ;
#13614 = CARTESIAN_POINT ( 'NONE',  ( 14.85437171138604207, -32.27599279215765904, 3.000000000000054179 ) ) ;
#13615 = DIRECTION ( 'NONE',  ( -0.000000000000000000, 1.000000000000000000, -0.000000000000000000 ) ) ;
#13616 = DIRECTION ( 'NONE',  ( 3.585095183685401065E-15, 0.000000000000000000, 1.000000000000000000 ) ) ;
#13617 = CIRCLE ( 'NONE', #14370, 34.90673715956759082 ) ;
#13618 = CARTESIAN_POINT ( 'NONE',  ( 19.99999999999998934, 18.38876824873586102, 60.62177826491085852 ) ) ;
#13619 = DIRECTION ( 'NONE',  ( -1.000000000000000000, 0.000000000000000000, 0.000000000000000000 ) ) ;
#13620 = EDGE_LOOP ( 'NONE', ( #10555, #5900, #10484, #20557, #14640, #15431, #3291, #9712 ) ) ;
#13621 = LINE ( 'NONE', #6779, #15687 ) ;
#13622 = CARTESIAN_POINT ( 'NONE',  ( -10.15869103000896345, 39.99999999999999289, -53.70409622859170895 ) ) ;
#13623 = ORIENTED_EDGE ( 'NONE', *, *, #4648, .T. ) ;
#13624 = EDGE_CURVE ( 'NONE', #5986, #4461, #17043, .T. ) ;
#13625 = CARTESIAN_POINT ( 'NONE',  ( -8.485281374238345720, 3.000000000000002665, -6.859353255829946150 ) ) ;
#13626 = AXIS2_PLACEMENT_3D ( 'NONE', #15713, #30, #17554 ) ;
#13627 = CARTESIAN_POINT ( 'NONE',  ( 1.942890293094023946E-13, -8.326672684688674053E-14, 4.999999999999993783 ) ) ;
#13628 = CARTESIAN_POINT ( 'NONE',  ( -13.56354382738803999, 2.142135623730931471, -56.03997097393684612 ) ) ;
#13629 = DIRECTION ( 'NONE',  ( -1.000000000000000000, 1.815202222194848078E-15, 0.000000000000000000 ) ) ;
#13630 = ORIENTED_EDGE ( 'NONE', *, *, #2047, .F. ) ;
#13631 = DIRECTION ( 'NONE',  ( -6.505213034913038160E-19, -3.903127820947822896E-18, -1.000000000000000000 ) ) ;
#13632 = VERTEX_POINT ( 'NONE', #14797 ) ;
#13633 = CARTESIAN_POINT ( 'NONE',  ( 10.49999999999994316, 42.51666049839543149, 60.00099999999999767 ) ) ;
#13634 = B_SPLINE_CURVE_WITH_KNOTS ( 'NONE', 3,
 ( #21295, #10618, #12453, #17623 ),
 .UNSPECIFIED., .F., .F.,
 ( 4, 4 ),
 ( 9.545285769942081322E-07, 0.001900595205834547038 ),
 .UNSPECIFIED. ) ;
#13635 = CARTESIAN_POINT ( 'NONE',  ( -21.93942599038056684, 24.73590942562832140, 58.56147853046847018 ) ) ;
#13636 = VERTEX_POINT ( 'NONE', #18598 ) ;
#13637 = CARTESIAN_POINT ( 'NONE',  ( -90.00000000000000000, 28.00000000000000000, 2.500000000000001332 ) ) ;
#13638 =( BOUNDED_SURFACE ( )  B_SPLINE_SURFACE ( 3, 2, ( 
 ( #8905, #15879, #17269 ),
 ( #193, #17727, #7308 ),
 ( #17615, #1922, #14158 ),
 ( #15544, #21176, #7074 ),
 ( #5476, #6863, #12447 ),
 ( #22570, #10723, #9021 ),
 ( #19119, #5256, #10387 ),
 ( #1705, #12231, #19235 ),
 ( #19460, #21286, #3545 ),
 ( #10502, #21861, #17844 ) ),
 .UNSPECIFIED., .F., .F., .F. ) 
 B_SPLINE_SURFACE_WITH_KNOTS ( ( 4, 2, 2, 2, 4 ),
 ( 3, 3 ),
 ( 0.02809317535148400657, 0.03071213539476974272, 0.03333109543805547886, 0.03595005548134121154, 0.03856901552462695115 ),
 ( 0.000000000000000000, 0.7610267056326938118 ),
 .UNSPECIFIED. ) 
 GEOMETRIC_REPRESENTATION_ITEM ( )  RATIONAL_B_SPLINE_SURFACE ( (
 ( 1.000000000000000000, 0.9420702913958448610, 0.9723126933862540344),
 ( 1.000000000000000000, 0.9476767737754007159, 0.9749922925143632568),
 ( 1.000000000000000000, 0.9527464803503639112, 0.9774153414777524418),
 ( 1.000000000000000000, 0.9613642323582910487, 0.9815341666525020381),
 ( 1.000000000000000000, 0.9649023417790275614, 0.9832251939807128416),
 ( 1.000000000000000000, 0.9700537923985854682, 0.9856873122313654090),
 ( 1.000000000000000000, 0.9716607116685208601, 0.9864553338148029926),
 ( 1.000000000000000000, 0.9729170072999735464, 0.9870557760262979041),
 ( 1.000000000000000000, 0.9725773074833657938, 0.9868934176577563999),
 ( 1.000000000000000000, 0.9714158944602965251, 0.9863383242652685734) ) ) 
 REPRESENTATION_ITEM ( '' )  SURFACE ( )  );
#13639 = CARTESIAN_POINT ( 'NONE',  ( 32.35999952201593288, -1.423424233832626395, -2.999999999999971578 ) ) ;
#13640 = ADVANCED_FACE ( 'NONE', ( #13291 ), #12208, .T. ) ;
#13641 = DIRECTION ( 'NONE',  ( 0.000000000000000000, 0.000000000000000000, -1.000000000000000000 ) ) ;
#13642 = VECTOR ( 'NONE', #1191, 1000.000000000000114 ) ;
#13643 = FACE_OUTER_BOUND ( 'NONE', #22604, .T. ) ;
#13644 = AXIS2_PLACEMENT_3D ( 'NONE', #16124, #14055, #17523 ) ;
#13645 = EDGE_CURVE ( 'NONE', #5630, #159, #18933, .T. ) ;
#13646 = CIRCLE ( 'NONE', #5273, 1.000000000000000888 ) ;
#13647 = ORIENTED_EDGE ( 'NONE', *, *, #16444, .F. ) ;
#13648 = ORIENTED_EDGE ( 'NONE', *, *, #1957, .F. ) ;
#13649 = ADVANCED_FACE ( 'NONE', ( #11933 ), #4847, .T. ) ;
#13650 = ORIENTED_EDGE ( 'NONE', *, *, #3319, .T. ) ;
#13651 = ORIENTED_EDGE ( 'NONE', *, *, #16529, .T. ) ;
#13652 = CARTESIAN_POINT ( 'NONE',  ( 2.775557561562891351E-14, 2.775557561562891351E-14, 5.750000000000001776 ) ) ;
#13653 = CARTESIAN_POINT ( 'NONE',  ( 18.32709649528715090, 33.00101640267666880, 57.63983358650816768 ) ) ;
#13654 = AXIS2_PLACEMENT_3D ( 'NONE', #8773, #1670, #15628 ) ;
#13655 = CARTESIAN_POINT ( 'NONE',  ( 9.952189117650862116, 40.00000000000000000, -53.64426396172072486 ) ) ;
#13656 = ORIENTED_EDGE ( 'NONE', *, *, #10439, .F. ) ;
#13657 = DIRECTION ( 'NONE',  ( -1.000000000000000000, -1.208970125616092456E-17, 0.000000000000000000 ) ) ;
#13658 = CARTESIAN_POINT ( 'NONE',  ( 0.7842774247521370201, 13.08102842795873677, 6.973256348136009031 ) ) ;
#13659 = ORIENTED_EDGE ( 'NONE', *, *, #21970, .F. ) ;
#13660 = FACE_OUTER_BOUND ( 'NONE', #12618, .T. ) ;
#13661 = AXIS2_PLACEMENT_3D ( 'NONE', #7649, #14620, #16227 ) ;
#13662 = ORIENTED_EDGE ( 'NONE', *, *, #331, .F. ) ;
#13663 = CARTESIAN_POINT ( 'NONE',  ( 5.833333333333329485, 39.00000000000000711, -40.61164310337066041 ) ) ;
#13664 = CIRCLE ( 'NONE', #1925, 2.500000000000002220 ) ;
#13665 = CARTESIAN_POINT ( 'NONE',  ( -35.00000000000000000, 15.00000000000000000, 41.00000000000002132 ) ) ;
#13666 = DIRECTION ( 'NONE',  ( -1.000000000000000000, 0.000000000000000000, 0.000000000000000000 ) ) ;
#13667 = CARTESIAN_POINT ( 'NONE',  ( -2.247171121184980525, 39.96957905804138278, 50.40104600615941166 ) ) ;
#13668=STYLED_ITEM('',(#22748),#10617);
#13669 = EDGE_CURVE ( 'NONE', #5811, #5141, #16674, .T. ) ;
#13670 = EDGE_CURVE ( 'NONE', #7488, #18483, #18819, .T. ) ;
#13671 = CARTESIAN_POINT ( 'NONE',  ( 0.000000000000000000, 10.00000000000000000, 0.000000000000000000 ) ) ;
#13672 = CARTESIAN_POINT ( 'NONE',  ( -42.50000000000000711, -9.600000000000001421, 47.50000000000000711 ) ) ;
#13673 = EDGE_CURVE ( 'NONE', #19784, #21644, #3357, .T. ) ;
#13674 = CIRCLE ( 'NONE', #15146, 16.49999999999998579 ) ;
#13675 = EDGE_LOOP ( 'NONE', ( #1208, #10526, #6938, #20134 ) ) ;
#13676 = VECTOR ( 'NONE', #3175, 1000.000000000000000 ) ;
#13677 = VERTEX_POINT ( 'NONE', #6671 ) ;
#13678 = ORIENTED_EDGE ( 'NONE', *, *, #21539, .T. ) ;
#13679 = CIRCLE ( 'NONE', #9267, 2.500000000000002220 ) ;
#13680 = EDGE_LOOP ( 'NONE', ( #906, #4279 ) ) ;
#13681 = CARTESIAN_POINT ( 'NONE',  ( -12.91716037299260122, 4.693711897366395824, 55.81219010901885724 ) ) ;
#13682 = CARTESIAN_POINT ( 'NONE',  ( -11.99035502499710937, 39.33333333333332860, 55.05149724789903587 ) ) ;
#13683 = CARTESIAN_POINT ( 'NONE',  ( -35.00000000000000000, 40.00000000000000000, -58.99999999999992895 ) ) ;
#13684 = DIRECTION ( 'NONE',  ( -0.000000000000000000, 1.000000000000000000, -0.000000000000000000 ) ) ;
#13685 = CARTESIAN_POINT ( 'NONE',  ( -12.01755860117731523, 39.99999999999999289, 54.34185968360770147 ) ) ;
#13686 = ORIENTED_EDGE ( 'NONE', *, *, #20469, .F. ) ;
#13687 = CARTESIAN_POINT ( 'NONE',  ( -42.50000000000000711, -9.600000000000001421, 45.00000000000000711 ) ) ;
#13688 = CARTESIAN_POINT ( 'NONE',  ( 34.99999999999980815, 40.00000000000000000, 57.49999999999921840 ) ) ;
#13689 = CARTESIAN_POINT ( 'NONE',  ( 35.00000000000001421, -5.000000000000000000, -4.999999999999997335 ) ) ;
#13690 = FACE_BOUND ( 'NONE', #15123, .T. ) ;
#13691 = DIRECTION ( 'NONE',  ( 0.000000000000000000, 0.000000000000000000, -1.000000000000000000 ) ) ;
#13692 = EDGE_CURVE ( 'NONE', #18082, #2079, #1402, .T. ) ;
#13693 = CIRCLE ( 'NONE', #8222, 50.00000000000000000 ) ;
#13694 = ORIENTED_EDGE ( 'NONE', *, *, #17824, .F. ) ;
#13695 = CARTESIAN_POINT ( 'NONE',  ( 6.123233995736766282E-16, -40.00000000000000000, -5.000000000000000000 ) ) ;
#13696 = ORIENTED_EDGE ( 'NONE', *, *, #740, .T. ) ;
#13697 = CARTESIAN_POINT ( 'NONE',  ( -13.06969024216331476, -19.15111107797470780, 2.999999999999995559 ) ) ;
#13698 = FACE_OUTER_BOUND ( 'NONE', #7184, .T. ) ;
#13699 = DIRECTION ( 'NONE',  ( -0.000000000000000000, -1.000000000000000000, 0.000000000000000000 ) ) ;
#13700 = DIRECTION ( 'NONE',  ( 0.000000000000000000, 0.000000000000000000, 1.000000000000000000 ) ) ;
#13701 = AXIS2_PLACEMENT_3D ( 'NONE', #20920, #5220, #11662 ) ;
#13702 = ORIENTED_EDGE ( 'NONE', *, *, #5495, .T. ) ;
#13703 = VECTOR ( 'NONE', #14629, 1000.000000000000000 ) ;
#13704 = CIRCLE ( 'NONE', #16956, 19.99999999999999289 ) ;
#13705 = EDGE_CURVE ( 'NONE', #14227, #22687, #15587, .T. ) ;
#13706 = ORIENTED_EDGE ( 'NONE', *, *, #22049, .F. ) ;
#13707 = CIRCLE ( 'NONE', #8608, 2.500000000000002220 ) ;
#13708 = CARTESIAN_POINT ( 'NONE',  ( -2.438270697430720446, -3.148887331866972783, 49.03407609142411872 ) ) ;
#13709 = DIRECTION ( 'NONE',  ( 0.000000000000000000, 0.000000000000000000, -1.000000000000000000 ) ) ;
#13710 = VERTEX_POINT ( 'NONE', #4954 ) ;
#13711 = EDGE_CURVE ( 'NONE', #17952, #1823, #4968, .T. ) ;
#13712 = DIRECTION ( 'NONE',  ( 6.505213034913038160E-19, 3.903127820947822896E-18, 1.000000000000000000 ) ) ;
#13713 = DIRECTION ( 'NONE',  ( -0.000000000000000000, -1.000000000000000000, -0.000000000000000000 ) ) ;
#13714 = CARTESIAN_POINT ( 'NONE',  ( -35.00000000000000000, 14.00000000000000000, 39.00000000000002132 ) ) ;
#13715 = AXIS2_PLACEMENT_3D ( 'NONE', #8951, #3703, #5195 ) ;
#13716 = CARTESIAN_POINT ( 'NONE',  ( -16.23901130407228166, 8.288052467681200852, -57.02826995000967258 ) ) ;
#13717 = DIRECTION ( 'NONE',  ( 0.000000000000000000, 0.000000000000000000, -1.000000000000000000 ) ) ;
#13718 = CIRCLE ( 'NONE', #14090, 2.499999999999996891 ) ;
#13719 = ORIENTED_EDGE ( 'NONE', *, *, #6475, .T. ) ;
#13720 = CARTESIAN_POINT ( 'NONE',  ( 8.188149873056865147, 32.58630821608365835, 42.20917188641859497 ) ) ;
#13721 = AXIS2_PLACEMENT_3D ( 'NONE', #16298, #9884, #18358 ) ;
#13722 = CARTESIAN_POINT ( 'NONE',  ( 35.00000000000000000, -5.000000000000000000, 57.49999999999698730 ) ) ;
#13723 = CARTESIAN_POINT ( 'NONE',  ( 42.50000000000000711, -5.000000000000000000, -47.50000000000000000 ) ) ;
#13724 = CIRCLE ( 'NONE', #19607, 58.99999999999994316 ) ;
#13725 = ORIENTED_EDGE ( 'NONE', *, *, #13017, .T. ) ;
#13726 = CARTESIAN_POINT ( 'NONE',  ( 7.558062341316965381E-15, -0.3324270965933701638, -47.91030067221370103 ) ) ;
#13727 = LINE ( 'NONE', #3100, #2884 ) ;
#13728 = AXIS2_PLACEMENT_3D ( 'NONE', #18356, #7944, #2676 ) ;
#13729 = EDGE_CURVE ( 'NONE', #16483, #5161, #10428, .T. ) ;
#13730 = EDGE_LOOP ( 'NONE', ( #16030, #21808 ) ) ;
#13731 = AXIS2_PLACEMENT_3D ( 'NONE', #18853, #20570, #3387 ) ;
#13732 = APPLICATION_PROTOCOL_DEFINITION ( 'draft international standard', 'automotive_design', 1998, #12230 ) ;
#13733 = EDGE_LOOP ( 'NONE', ( #4796, #22375, #13757, #9850 ) ) ;
#13734 = DIRECTION ( 'NONE',  ( -0.000000000000000000, -1.000000000000000000, -0.000000000000000000 ) ) ;
#13735 = EDGE_CURVE ( 'NONE', #12221, #1729, #21798, .T. ) ;
#13736 = CIRCLE ( 'NONE', #16690, 18.42595423422130452 ) ;
#13737 = DIRECTION ( 'NONE',  ( 1.296372316667914327E-16, 1.000000000000000000, -0.000000000000000000 ) ) ;
#13738 = DIRECTION ( 'NONE',  ( 0.000000000000000000, 0.000000000000000000, -1.000000000000000000 ) ) ;
#13739 = DIRECTION ( 'NONE',  ( 0.000000000000000000, 0.000000000000000000, 1.000000000000000000 ) ) ;
#13740 = CARTESIAN_POINT ( 'NONE',  ( -7.463862311151175710, -35.99819890246952525, -2.800654218530457484 ) ) ;
#13741 = EDGE_LOOP ( 'NONE', ( #20474, #18366, #21710, #11436 ) ) ;
#13742 = DIRECTION ( 'NONE',  ( -0.000000000000000000, -0.000000000000000000, 1.000000000000000000 ) ) ;
#13743 = FACE_OUTER_BOUND ( 'NONE', #11198, .T. ) ;
#13744 = ORIENTED_EDGE ( 'NONE', *, *, #12557, .F. ) ;
#13745 = CARTESIAN_POINT ( 'NONE',  ( -42.50000000000000711, -11.97499999999999964, 45.00000000000000711 ) ) ;
#13746 = CARTESIAN_POINT ( 'NONE',  ( -14.93538271375417814, -34.13396246814587442, -6.999999999999950262 ) ) ;
#13747 = CARTESIAN_POINT ( 'NONE',  ( -35.00000000000000000, 40.00000000000000000, 1.387778780781445676E-14 ) ) ;
#13748 = DIRECTION ( 'NONE',  ( 6.505213034913038160E-19, 3.903127820947822896E-18, 1.000000000000000000 ) ) ;
#13749 = DIRECTION ( 'NONE',  ( -1.000000000000000000, 0.000000000000000000, 0.000000000000000000 ) ) ;
#13750 = ORIENTED_EDGE ( 'NONE', *, *, #7636, .T. ) ;
#13751 = DIRECTION ( 'NONE',  ( -0.000000000000000000, -1.000000000000000000, -0.000000000000000000 ) ) ;
#13752 = AXIS2_PLACEMENT_3D ( 'NONE', #15128, #2908, #15361 ) ;
#13753 = CIRCLE ( 'NONE', #2808, 2.499999999999998668 ) ;
#13754 = DIRECTION ( 'NONE',  ( 6.505213034913038160E-19, 3.903127820947822896E-18, 1.000000000000000000 ) ) ;
#13755 = CIRCLE ( 'NONE', #16322, 2.499999999999995115 ) ;
#13756 = VECTOR ( 'NONE', #19134, 1000.000000000000000 ) ;
#13757 = ORIENTED_EDGE ( 'NONE', *, *, #15688, .T. ) ;
#13758 = FACE_OUTER_BOUND ( 'NONE', #21427, .T. ) ;
#13759 = EDGE_CURVE ( 'NONE', #10311, #21906, #6119, .T. ) ;
#13760 = FACE_OUTER_BOUND ( 'NONE', #15772, .T. ) ;
#13761 = DIRECTION ( 'NONE',  ( -1.000000000000000000, -1.208970125616081209E-17, 0.000000000000000000 ) ) ;
#13762 = CIRCLE ( 'NONE', #617, 2.525000000000110489 ) ;
#13763 = CARTESIAN_POINT ( 'NONE',  ( -1.387778780781445518E-14, 20.00000000000000355, -105.0000000000000142 ) ) ;
#13764 = EDGE_CURVE ( 'NONE', #19146, #121, #9252, .T. ) ;
#13765 = EDGE_CURVE ( 'NONE', #7904, #7, #3583, .T. ) ;
#13766 = ORIENTED_EDGE ( 'NONE', *, *, #9948, .T. ) ;
#13767 = EDGE_LOOP ( 'NONE', ( #8715, #15359, #2552, #4552 ) ) ;
#13768 = EDGE_LOOP ( 'NONE', ( #17092, #7145, #20769, #7101 ) ) ;
#13769 = CARTESIAN_POINT ( 'NONE',  ( -12.31876324338271367, -30.07487443287973505, -2.999999999999995559 ) ) ;
#13770 = AXIS2_PLACEMENT_3D ( 'NONE', #7457, #21560, #4479 ) ;
#13771 = ORIENTED_EDGE ( 'NONE', *, *, #12786, .F. ) ;
#13772 = DIRECTION ( 'NONE',  ( 1.000000000000000000, 0.000000000000000000, 0.000000000000000000 ) ) ;
#13773 = CARTESIAN_POINT ( 'NONE',  ( -13.00000000000011546, 42.51666049839536043, -105.0000000000000142 ) ) ;
#13774 = PLANE ( 'NONE',  #15395 ) ;
#13775 = ADVANCED_FACE ( 'NONE', ( #11320 ), #18917, .T. ) ;
#13776 = ORIENTED_EDGE ( 'NONE', *, *, #9112, .F. ) ;
#13777 = PLANE ( 'NONE',  #18606 ) ;
#13778 = CARTESIAN_POINT ( 'NONE',  ( -0.2227364088731864089, -1.232651810764356037, -48.42315971483976966 ) ) ;
#13779 = ORIENTED_EDGE ( 'NONE', *, *, #17613, .F. ) ;
#13780 = CARTESIAN_POINT ( 'NONE',  ( -3.313694450323563689, 0.2469464189807611398, 51.08096178187792447 ) ) ;
#13781 = CIRCLE ( 'NONE', #10122, 51.00000000000002132 ) ;
#13782 = CARTESIAN_POINT ( 'NONE',  ( 2.095812652544434496, 34.85510830401392468, 38.95253985045414424 ) ) ;
#13783 = ORIENTED_EDGE ( 'NONE', *, *, #14606, .T. ) ;
#13784 = CARTESIAN_POINT ( 'NONE',  ( 8.123113521816467397, 39.63127166633003640, -53.85467626787994533 ) ) ;
#13785 = ADVANCED_FACE ( 'NONE', ( #429 ), #890, .F. ) ;
#13786 = LINE ( 'NONE', #1436, #2511 ) ;
#13787 = DIRECTION ( 'NONE',  ( 6.505213034913038160E-19, 3.903127820947822896E-18, 1.000000000000000000 ) ) ;
#13788 = CARTESIAN_POINT ( 'NONE',  ( -0.4976657361290892090, 39.99853738388662805, 49.11742177756252659 ) ) ;
#13789 = ADVANCED_FACE ( 'NONE', ( #16582 ), #12271, .T. ) ;
#13790 = CIRCLE ( 'NONE', #4671, 1.000000000000000888 ) ;
#13791 = CARTESIAN_POINT ( 'NONE',  ( -21.05198877411783442, 30.13956425491229396, -2.800654218530457484 ) ) ;
#13792 = CARTESIAN_POINT ( 'NONE',  ( -1.128083539116059297, -34.88850421923977763, 2.999999999999995559 ) ) ;
#13793 = EDGE_CURVE ( 'NONE', #19871, #18308, #16357, .T. ) ;
#13794 = ORIENTED_EDGE ( 'NONE', *, *, #1082, .T. ) ;
#13795 = ORIENTED_EDGE ( 'NONE', *, *, #15325, .F. ) ;
#13796 = AXIS2_PLACEMENT_3D ( 'NONE', #227, #3460, #7218 ) ;
#13797 = VERTEX_POINT ( 'NONE', #19807 ) ;
#13798 = EDGE_CURVE ( 'NONE', #3722, #10477, #366, .T. ) ;
#13799 = ORIENTED_EDGE ( 'NONE', *, *, #3680, .T. ) ;
#13800 = CARTESIAN_POINT ( 'NONE',  ( 90.00000000000000000, 26.00000000000000355, -9.108981535246192915E-16 ) ) ;
#13801 = CARTESIAN_POINT ( 'NONE',  ( -37.07861450834793970, 3.656418565264024423, -2.999999999999988898 ) ) ;
#13802 = AXIS2_PLACEMENT_3D ( 'NONE', #2562, #17792, #19632 ) ;
#13803 = AXIS2_PLACEMENT_3D ( 'NONE', #6727, #3410, #10372 ) ;
#13804 = ADVANCED_FACE ( 'NONE', ( #19914 ), #7659, .F. ) ;
#13805 = CARTESIAN_POINT ( 'NONE',  ( -3.469446951953614189E-14, -1.000000000000028644, 48.73397172404114031 ) ) ;
#13806 = CARTESIAN_POINT ( 'NONE',  ( 4.273192510725268178, 39.88698591164679641, 51.75894906208631596 ) ) ;
#13807 = CIRCLE ( 'NONE', #5052, 0.9999999999999991118 ) ;
#13808 = ORIENTED_EDGE ( 'NONE', *, *, #10227, .F. ) ;
#13809 = CARTESIAN_POINT ( 'NONE',  ( 2.220446049250313081E-13, -2.498001805406602216E-13, -6.859353255829918616 ) ) ;
#13810 = LINE ( 'NONE', #13348, #12661 ) ;
#13811 = DIRECTION ( 'NONE',  ( -0.000000000000000000, 1.000000000000000000, -0.000000000000000000 ) ) ;
#13812 = DIRECTION ( 'NONE',  ( -0.000000000000000000, 1.000000000000000000, -0.000000000000000000 ) ) ;
#13813 = PRESENTATION_STYLE_ASSIGNMENT (( #15529 ) ) ;
#13814 = ORIENTED_EDGE ( 'NONE', *, *, #14399, .T. ) ;
#13815 = DIRECTION ( 'NONE',  ( -6.505213034913038160E-19, -3.903127820947822896E-18, -1.000000000000000000 ) ) ;
#13816 = AXIS2_PLACEMENT_3D ( 'NONE', #6085, #11013, #7798 ) ;
#13817 = CARTESIAN_POINT ( 'NONE',  ( -20.00000000000001421, 20.97067337953453858, 60.62177826491070221 ) ) ;
#13818 = VERTEX_POINT ( 'NONE', #11196 ) ;
#13819 = CARTESIAN_POINT ( 'NONE',  ( -1.128083539116059297, -34.88850421923977763, 2.999999999999995559 ) ) ;
#13820 = VECTOR ( 'NONE', #17909, 1000.000000000000000 ) ;
#13821 = CIRCLE ( 'NONE', #1757, 2.500000000000002220 ) ;
#13822 = DIRECTION ( 'NONE',  ( 0.000000000000000000, -0.000000000000000000, 1.000000000000000000 ) ) ;
#13823 = FACE_OUTER_BOUND ( 'NONE', #17901, .T. ) ;
#13824 = CARTESIAN_POINT ( 'NONE',  ( 3.330669073875469621E-13, -1.110223024625156540E-13, -2.999999999999971578 ) ) ;
#13825 = AXIS2_PLACEMENT_3D ( 'NONE', #20582, #13341, #22323 ) ;
#13826 = ORIENTED_EDGE ( 'NONE', *, *, #7776, .F. ) ;
#13827 = ADVANCED_FACE ( 'NONE', ( #782 ), #19277, .T. ) ;
#13828 = VERTEX_POINT ( 'NONE', #9494 ) ;
#13829 = DIRECTION ( 'NONE',  ( -1.000000000000000000, -1.208970125616046080E-17, 6.505213034913038160E-19 ) ) ;
#13830 = CONICAL_SURFACE ( 'NONE', #19353, 59.99999999999700862, 0.7853981633974380649 ) ;
#13831 = CARTESIAN_POINT ( 'NONE',  ( 35.33352588067112521, 7.094908322882925944, -6.999999999999999112 ) ) ;
#13832 = ORIENTED_EDGE ( 'NONE', *, *, #5039, .F. ) ;
#13833 = VECTOR ( 'NONE', #15274, 1000.000000000000000 ) ;
#13834 = CARTESIAN_POINT ( 'NONE',  ( 12.68897045256288258, 11.99170770793158525, 44.74667050109238176 ) ) ;
#13835 = ADVANCED_FACE ( 'NONE', ( #17852 ), #21857, .F. ) ;
#13836 = CARTESIAN_POINT ( 'NONE',  ( -4.985660570713215556, 34.15523982581864715, -40.05045397208977676 ) ) ;
#13837 = DIRECTION ( 'NONE',  ( -1.000000000000000000, 0.000000000000000000, 0.000000000000000000 ) ) ;
#13838 = CARTESIAN_POINT ( 'NONE',  ( -21.98712579307494508, 15.48449832073882781, -58.57208548029186801 ) ) ;
#13839 = VECTOR ( 'NONE', #13860, 1000.000000000000000 ) ;
#13840 = CARTESIAN_POINT ( 'NONE',  ( -14.76055860720891033, 22.69766935715934508, -45.72055682016588918 ) ) ;
#13841 = VERTEX_POINT ( 'NONE', #21751 ) ;
#13842 = DIRECTION ( 'NONE',  ( 0.000000000000000000, 0.000000000000000000, -1.000000000000000000 ) ) ;
#13843 = DIRECTION ( 'NONE',  ( -0.000000000000000000, 1.000000000000000000, -0.000000000000000000 ) ) ;
#13844 = CARTESIAN_POINT ( 'NONE',  ( 13.00000000000000178, -20.00000000000000000, -11.32475165290605901 ) ) ;
#13845 = VERTEX_POINT ( 'NONE', #5706 ) ;
#13846 = COLOUR_RGB ( '',0.7921568627450980005, 0.8196078431372548767, 0.9333333333333333481 ) ;
#13847 = CARTESIAN_POINT ( 'NONE',  ( -16.56444186175072630, 26.79308242454869671, -6.999999999999950262 ) ) ;
#13848 = CARTESIAN_POINT ( 'NONE',  ( -42.49999999999996447, 7.000000000000000000, -47.50000000000000711 ) ) ;
#13849 = CIRCLE ( 'NONE', #20090, 9.000000000000003553 ) ;
#13850 = EDGE_CURVE ( 'NONE', #16688, #2421, #6048, .T. ) ;
#13851 = DIRECTION ( 'NONE',  ( 1.000000000000000000, 0.000000000000000000, 0.000000000000000000 ) ) ;
#13852 = EDGE_LOOP ( 'NONE', ( #21637, #1918, #18770, #1649, #15295, #6583, #9900, #16591, #18384, #10692 ) ) ;
#13853 = APPLICATION_PROTOCOL_DEFINITION ( 'draft international standard', 'automotive_design', 1998, #5637 ) ;
#13854 = VERTEX_POINT ( 'NONE', #10973 ) ;
#13855 = DIRECTION ( 'NONE',  ( -6.505213034913038160E-19, -3.903127820947822896E-18, -1.000000000000000000 ) ) ;
#13856 = DIRECTION ( 'NONE',  ( -1.000000000000000000, -1.815202222194848473E-15, 0.000000000000000000 ) ) ;
#13857 = DIRECTION ( 'NONE',  ( 0.000000000000000000, -1.000000000000000000, 0.000000000000000000 ) ) ;
#13858 = CARTESIAN_POINT ( 'NONE',  ( -42.50000000000000711, -5.000000000000000000, -54.00000000000000000 ) ) ;
#13859 = CIRCLE ( 'NONE', #13494, 36.76383501243555685 ) ;
#13860 = DIRECTION ( 'NONE',  ( -0.000000000000000000, -1.000000000000000000, -0.000000000000000000 ) ) ;
#13861 = ORIENTED_EDGE ( 'NONE', *, *, #5392, .F. ) ;
#13862 = DIRECTION ( 'NONE',  ( 0.000000000000000000, -1.000000000000000000, 0.000000000000000000 ) ) ;
#13863 = DIRECTION ( 'NONE',  ( 6.505213034913038160E-19, 3.903127820947822896E-18, 1.000000000000000000 ) ) ;
#13864 = ORIENTED_EDGE ( 'NONE', *, *, #2014, .T. ) ;
#13865 = CARTESIAN_POINT ( 'NONE',  ( 7.776554266669417956E-15, -4.648749848372173865, -45.43309249825056639 ) ) ;
#13866 = CARTESIAN_POINT ( 'NONE',  ( 21.73016838732307576, 25.62687619368169223, -58.51481333197131818 ) ) ;
#13867 = DIRECTION ( 'NONE',  ( 0.1421319796954322034, 0.000000000000000000, -0.9898477157360405787 ) ) ;
#13868 = CARTESIAN_POINT ( 'NONE',  ( -7.474679935337165126, 39.63145871004727638, -53.58934899115953243 ) ) ;
#13869 = ORIENTED_EDGE ( 'NONE', *, *, #10439, .T. ) ;
#13870 = DIRECTION ( 'NONE',  ( 0.000000000000000000, 0.000000000000000000, 1.000000000000000000 ) ) ;
#13871 = CARTESIAN_POINT ( 'NONE',  ( 6.696867368503558448E-15, 40.00000000000000000, 48.73397172404481381 ) ) ;
#13872 = ADVANCED_FACE ( 'NONE', ( #16819 ), #13365, .T. ) ;
#13873 = ORIENTED_EDGE ( 'NONE', *, *, #4537, .F. ) ;
#13874 = CARTESIAN_POINT ( 'NONE',  ( 42.49999999999998579, 7.000000000000000000, -47.49999999999997868 ) ) ;
#13875 = PRODUCT_RELATED_PRODUCT_CATEGORY ( 'part', '', ( #8039 ) ) ;
#13876 = CARTESIAN_POINT ( 'NONE',  ( 89.99999999999701572, -5.000000000000000000, -2.500000000000060840 ) ) ;
#13877 = CARTESIAN_POINT ( 'NONE',  ( -24.99999999999999645, -20.00000000000000000, 25.00000000000001421 ) ) ;
#13878 = CARTESIAN_POINT ( 'NONE',  ( 35.00000000000058265, 26.00000000000000355, -57.10000000000076170 ) ) ;
#13879 = VECTOR ( 'NONE', #9935, 1000.000000000000000 ) ;
#13880 = ORIENTED_EDGE ( 'NONE', *, *, #17983, .T. ) ;
#13881 = EDGE_LOOP ( 'NONE', ( #13207, #17570, #14812, #13894 ) ) ;
#13882 = ORIENTED_EDGE ( 'NONE', *, *, #17010, .T. ) ;
#13883 = DIRECTION ( 'NONE',  ( 1.296372316667914327E-16, 1.000000000000000000, -0.000000000000000000 ) ) ;
#13884 = VERTEX_POINT ( 'NONE', #20862 ) ;
#13885 = CARTESIAN_POINT ( 'NONE',  ( 36.39375341857550694, 7.980461308159797262, -6.999999999999971578 ) ) ;
#13886 = CARTESIAN_POINT ( 'NONE',  ( 18.74703631669234127, 7.639653230112233295, 57.75728470191489805 ) ) ;
#13887 = CIRCLE ( 'NONE', #4045, 19.11328065563150957 ) ;
#13888 = CARTESIAN_POINT ( 'NONE',  ( 6.000000000000000000, 20.00000000000000000, 5.999999999999999112 ) ) ;
#13889 = CARTESIAN_POINT ( 'NONE',  ( 4.643077362641815142, 40.00000000000000711, 51.42938339147494275 ) ) ;
#13890 = EDGE_CURVE ( 'NONE', #21191, #12680, #17405, .T. ) ;
#13891 = ORIENTED_EDGE ( 'NONE', *, *, #20725, .F. ) ;
#13892 = DIRECTION ( 'NONE',  ( -0.000000000000000000, -1.000000000000000000, -0.000000000000000000 ) ) ;
#13893 = CARTESIAN_POINT ( 'NONE',  ( 2.220446049250313081E-13, 2.775557561562891351E-14, -2.800654218530485018 ) ) ;
#13894 = ORIENTED_EDGE ( 'NONE', *, *, #6921, .F. ) ;
#13895 = CARTESIAN_POINT ( 'NONE',  ( 1.110223024625156540E-13, -5.551115123125782702E-14, -6.999999999999950262 ) ) ;
#13896 = AXIS2_PLACEMENT_3D ( 'NONE', #20194, #12843, #4057 ) ;
#13897 = LINE ( 'NONE', #15618, #3615 ) ;
#13898 = EDGE_LOOP ( 'NONE', ( #10430, #3564, #257, #15132, #7698, #21790, #21674, #7985, #17793 ) ) ;
#13899 = CARTESIAN_POINT ( 'NONE',  ( 1.734786545154649763E-13, -1.500000000000015099, -16.00000000000029488 ) ) ;
#13900 = EDGE_CURVE ( 'NONE', #11717, #17625, #19250, .T. ) ;
#13901 = CARTESIAN_POINT ( 'NONE',  ( -6.401811138932623990, 38.95166772950821610, 55.13648753466793551 ) ) ;
#13902 = CARTESIAN_POINT ( 'NONE',  ( -4.274778969419686270, 39.88689869269535393, 51.75995440011182325 ) ) ;
#13903 = DIRECTION ( 'NONE',  ( -6.505213034913038160E-19, -3.903127820947822896E-18, -1.000000000000000000 ) ) ;
#13904 = FACE_BOUND ( 'NONE', #22080, .T. ) ;
#13905 = AXIS2_PLACEMENT_3D ( 'NONE', #12083, #15731, #8526 ) ;
#13906 = CARTESIAN_POINT ( 'NONE',  ( -90.00000000000000000, 28.00000000000000000, -9.108981535246192915E-16 ) ) ;
#13907 = ORIENTED_EDGE ( 'NONE', *, *, #20821, .T. ) ;
#13908 = ORIENTED_EDGE ( 'NONE', *, *, #21649, .F. ) ;
#13909 = ORIENTED_EDGE ( 'NONE', *, *, #6122, .F. ) ;
#13910 = ORIENTED_EDGE ( 'NONE', *, *, #4506, .F. ) ;
#13911 = DIRECTION ( 'NONE',  ( -1.000000000000000000, 2.663326288974754901E-14, 0.000000000000000000 ) ) ;
#13912 = DIRECTION ( 'NONE',  ( 0.000000000000000000, 0.000000000000000000, -1.000000000000000000 ) ) ;
#13913 = EDGE_CURVE ( 'NONE', #17042, #11377, #7096, .T. ) ;
#13914 = CARTESIAN_POINT ( 'NONE',  ( -10.34137811700568932, 39.99999999999998579, -53.75702834151140763 ) ) ;
#13915 = CARTESIAN_POINT ( 'NONE',  ( 5.551115123125782702E-14, -1.387778780781445676E-13, -5.749999999999949374 ) ) ;
#13916 = CARTESIAN_POINT ( 'NONE',  ( 5.042540895202911599, 39.84191929402975774, 52.23966295474247090 ) ) ;
#13917 = ORIENTED_EDGE ( 'NONE', *, *, #17385, .F. ) ;
#13918 = CARTESIAN_POINT ( 'NONE',  ( -34.64233806479151667, -10.34893680499436819, 2.932969818539049811 ) ) ;
#13919 = CARTESIAN_POINT ( 'NONE',  ( 35.00000000000000000, 2.142135623730931471, 4.258610482196280173E-15 ) ) ;
#13920 = EDGE_CURVE ( 'NONE', #14529, #10205, #8925, .T. ) ;
#13921 = CARTESIAN_POINT ( 'NONE',  ( -0.8499999999999410250, -5.000000000000000000, -48.11213464397154382 ) ) ;
#13922 = EDGE_CURVE ( 'NONE', #2563, #4860, #2052, .T. ) ;
#13923 = CARTESIAN_POINT ( 'NONE',  ( 10.72803533576303359, 40.00000000000000711, -53.87712872072452797 ) ) ;
#13924 = DIRECTION ( 'NONE',  ( -1.000000000000000000, 0.000000000000000000, 0.000000000000000000 ) ) ;
#13925 = VERTEX_POINT ( 'NONE', #19585 ) ;
#13926 = CARTESIAN_POINT ( 'NONE',  ( -7.524443153164583897, 20.67323765728967899, 2.999999999999992450 ) ) ;
#13927 = DIRECTION ( 'NONE',  ( 0.000000000000000000, 0.000000000000000000, 1.000000000000000000 ) ) ;
#13928 = CARTESIAN_POINT ( 'NONE',  ( -48.93401015228422324, 10.00000000000000000, -46.57614213197970088 ) ) ;
#13929 = EDGE_CURVE ( 'NONE', #15217, #10145, #20352, .T. ) ;
#13930 = ORIENTED_EDGE ( 'NONE', *, *, #14943, .T. ) ;
#13931 = ORIENTED_EDGE ( 'NONE', *, *, #8717, .F. ) ;
#13932 = VERTEX_POINT ( 'NONE', #17527 ) ;
#13933 = DIRECTION ( 'NONE',  ( 0.000000000000000000, -1.000000000000000000, 0.000000000000000000 ) ) ;
#13934 = CARTESIAN_POINT ( 'NONE',  ( 11.13570271988770877, 40.00000000000000711, -54.01634158485467907 ) ) ;
#13935 = VERTEX_POINT ( 'NONE', #5383 ) ;
#13936 = AXIS2_PLACEMENT_3D ( 'NONE', #22480, #4832, #18806 ) ;
#13937 = FACE_BOUND ( 'NONE', #11833, .T. ) ;
#13938 = CARTESIAN_POINT ( 'NONE',  ( -1.833353995796109137, 34.88982467546053812, -38.89995731584649974 ) ) ;
#13939 = FACE_OUTER_BOUND ( 'NONE', #15594, .T. ) ;
#13940 = CARTESIAN_POINT ( 'NONE',  ( -20.00279574339814559, 20.27588806490366125, -58.14815718763279762 ) ) ;
#13941 = DIRECTION ( 'NONE',  ( -0.000000000000000000, 1.000000000000000000, -0.000000000000000000 ) ) ;
#13942 = VERTEX_POINT ( 'NONE', #1837 ) ;
#13943 = CARTESIAN_POINT ( 'NONE',  ( -34.99999999999980815, 28.00000000000000000, 57.49999999999921840 ) ) ;
#13944 = PLANE ( 'NONE',  #5281 ) ;
#13945 = DIRECTION ( 'NONE',  ( 1.000000000000000000, 1.208970125616065955E-17, 0.000000000000000000 ) ) ;
#13946 = DIRECTION ( 'NONE',  ( -6.505213034913038160E-19, -3.903127820947822896E-18, -1.000000000000000000 ) ) ;
#13947 = EDGE_CURVE ( 'NONE', #249, #9389, #12284, .T. ) ;
#13948 = ORIENTED_EDGE ( 'NONE', *, *, #2028, .T. ) ;
#13949 = EDGE_CURVE ( 'NONE', #12221, #2570, #1938, .T. ) ;
#13950 = DIRECTION ( 'NONE',  ( 6.505213034913038160E-19, 3.903127820947822896E-18, 1.000000000000000000 ) ) ;
#13951 = VECTOR ( 'NONE', #21558, 1000.000000000000000 ) ;
#13952 = EDGE_CURVE ( 'NONE', #19883, #11772, #22589, .T. ) ;
#13953 = ORIENTED_EDGE ( 'NONE', *, *, #22437, .T. ) ;
#13954 = EDGE_LOOP ( 'NONE', ( #16989, #9764, #16502, #12060, #12446, #21890 ) ) ;
#13955 = CARTESIAN_POINT ( 'NONE',  ( 3.330669073875469621E-13, -1.110223024625156540E-13, -2.999999999999971578 ) ) ;
#13956 = CARTESIAN_POINT ( 'NONE',  ( 6.976853941411403248, 1.175947842326362069, -53.23020196595923181 ) ) ;
#13957 = DIRECTION ( 'NONE',  ( 0.000000000000000000, 0.000000000000000000, 1.000000000000000000 ) ) ;
#13958 = FACE_OUTER_BOUND ( 'NONE', #12176, .T. ) ;
#13959 = DIRECTION ( 'NONE',  ( 0.000000000000000000, -0.000000000000000000, -1.000000000000000000 ) ) ;
#13960 = ORIENTED_EDGE ( 'NONE', *, *, #20012, .F. ) ;
#13961 = CARTESIAN_POINT ( 'NONE',  ( -36.76383501243539342, 2.727773753693014013E-14, -2.800654218530485018 ) ) ;
#13962 = DIRECTION ( 'NONE',  ( -1.000000000000000000, 1.815202222194848473E-15, 0.000000000000000000 ) ) ;
#13963 = ORIENTED_EDGE ( 'NONE', *, *, #3868, .T. ) ;
#13964 = CARTESIAN_POINT ( 'NONE',  ( 4.153516728483875653, -35.28654656445792170, 3.000000000000031974 ) ) ;
#13965 = CARTESIAN_POINT ( 'NONE',  ( 21.20802570598056036, 27.37171784732025515, -58.39394879075534561 ) ) ;
#13966 = AXIS2_PLACEMENT_3D ( 'NONE', #8781, #15635, #13911 ) ;
#13967 = DIRECTION ( 'NONE',  ( 0.000000000000000000, 0.000000000000000000, 1.000000000000000000 ) ) ;
#13968 = CARTESIAN_POINT ( 'NONE',  ( 8.197131407637472833, 40.00000000000000711, 53.04141934721033635 ) ) ;
#13969 = CARTESIAN_POINT ( 'NONE',  ( 12.70473862104218021, 28.00863069209355416, -44.75655646380167951 ) ) ;
#13970 = VERTEX_POINT ( 'NONE', #9041 ) ;
#13971 = LINE ( 'NONE', #20889, #8285 ) ;
#13972 = CARTESIAN_POINT ( 'NONE',  ( -19.23435001722038251, 8.416038526954890742, 57.89219688981300749 ) ) ;
#13973 = ORIENTED_EDGE ( 'NONE', *, *, #4579, .T. ) ;
#13974 = DIRECTION ( 'NONE',  ( -6.505213034913038160E-19, -3.903127820947822896E-18, -1.000000000000000000 ) ) ;
#13975 = DIRECTION ( 'NONE',  ( -1.000000000000000000, 0.000000000000000000, 0.000000000000000000 ) ) ;
#13976 = VERTEX_POINT ( 'NONE', #21303 ) ;
#13977 = ORIENTED_EDGE ( 'NONE', *, *, #5661, .F. ) ;
#13978 = VERTEX_POINT ( 'NONE', #100 ) ;
#13979 = FACE_BOUND ( 'NONE', #7602, .T. ) ;
#13980 = AXIS2_PLACEMENT_3D ( 'NONE', #14921, #21826, #20447 ) ;
#13981 = EDGE_CURVE ( 'NONE', #16002, #9114, #18152, .T. ) ;
#13982 = EDGE_LOOP ( 'NONE', ( #14478, #1385, #5475, #10932, #6685, #19620, #22452, #13001 ) ) ;
#13983 = CARTESIAN_POINT ( 'NONE',  ( 35.00000000000001421, 1.000000000000044187, 10.00000000000000000 ) ) ;
#13984 = CARTESIAN_POINT ( 'NONE',  ( 35.00000000000001421, 0.000000000000000000, 1.540743955509788682E-30 ) ) ;
#13985 = CARTESIAN_POINT ( 'NONE',  ( 8.743619455145315911, 40.00000000000000711, 53.24632774152720316 ) ) ;
#13986 = ORIENTED_EDGE ( 'NONE', *, *, #15105, .T. ) ;
#13987 = FACE_BOUND ( 'NONE', #3962, .T. ) ;
#13988 = CARTESIAN_POINT ( 'NONE',  ( -30.33632613426172497, 11.35354668330676375, -2.999999999999988898 ) ) ;
#13989 = ORIENTED_EDGE ( 'NONE', *, *, #17497, .T. ) ;
#13990 = CARTESIAN_POINT ( 'NONE',  ( -5.833333333333337478, 6.180730040185833829, -40.61164310337066041 ) ) ;
#13991 = CARTESIAN_POINT ( 'NONE',  ( -8.566020585660502861E-14, -3.670992598665648643, 46.55272505131122074 ) ) ;
#13992 = EDGE_CURVE ( 'NONE', #11767, #2030, #19140, .T. ) ;
#13993 = ORIENTED_EDGE ( 'NONE', *, *, #5497, .T. ) ;
#13994 = CARTESIAN_POINT ( 'NONE',  ( -47.83731665821558465, 10.00000000000000000, 38.93845529828710283 ) ) ;
#13995 = EDGE_LOOP ( 'NONE', ( #21282, #3710, #13455, #4683, #13766, #4385 ) ) ;
#13996 = DIRECTION ( 'NONE',  ( -6.505213034913038160E-19, -3.903127820947822896E-18, -1.000000000000000000 ) ) ;
#13997 = CARTESIAN_POINT ( 'NONE',  ( 19.05255888325763181, 11.00000000000003730, -2.999999999999971578 ) ) ;
#13998 = LINE ( 'NONE', #10581, #17172 ) ;
#13999 = CIRCLE ( 'NONE', #5973, 17.00000000000001421 ) ;
#14000 = B_SPLINE_CURVE_WITH_KNOTS ( 'NONE', 3,
 ( #9209, #16187, #496, #7495, #10680, #8981, #15962, #12000, #22000, #8020, #14978, #11099, #7781, #9511, #14534, #18091, #21545, #2525, #13150, #13031, #5843, #11338, #9727, #6292, #18323, #12810, #9612, #7901, #14646, #6186, #798, #14755, #20163, #2405, #12920, #4583, #4238, #18213, #21770, #11562, #14864 ),
 .UNSPECIFIED., .F., .F.,
 ( 4, 1, 1, 1, 1, 2, 2, 1, 1, 1, 1, 2, 2, 1, 1, 1, 2, 2, 1, 1, 1, 2, 2, 1, 1, 1, 2, 2, 4 ),
 ( 0.000000000000000000, 0.06250000000000577316, 0.09375000000000836831, 0.1093750000000093675, 0.1171875000000101585, 0.1210937500000100614, 0.1250000000000099643, 0.1875000000000074385, 0.2187500000000063283, 0.2343750000000055234, 0.2421875000000053568, 0.2460937500000053846, 0.2500000000000053846, 0.3125000000000038858, 0.3437500000000032196, 0.3593750000000023870, 0.3671875000000019984, 0.3750000000000016098, 0.4375000000000014433, 0.4687500000000018874, 0.4843750000000021094, 0.4921875000000017208, 0.5000000000000013323, 0.6249999999999993339, 0.6874999999999983347, 0.7187499999999977796, 0.7343749999999975575, 0.7499999999999973355, 1.000000000000000000 ),
 .UNSPECIFIED. ) ;
#14001 = CARTESIAN_POINT ( 'NONE',  ( 19.02718446893024407, 26.17927818497044612, 57.88297158504753526 ) ) ;
#14002 = LINE ( 'NONE', #1890, #20240 ) ;
#14003 = TOROIDAL_SURFACE ( 'NONE', #11472, 18.00000000000000355, 4.000000000000000000 ) ;
#14004 = CIRCLE ( 'NONE', #5596, 39.00000000000000000 ) ;
#14005 = DIRECTION ( 'NONE',  ( -0.000000000000000000, -0.000000000000000000, -1.000000000000000000 ) ) ;
#14006 = ORIENTED_EDGE ( 'NONE', *, *, #19445, .T. ) ;
#14007 = ORIENTED_EDGE ( 'NONE', *, *, #1422, .F. ) ;
#14008 = AXIS2_PLACEMENT_3D ( 'NONE', #5910, #13105, #21380 ) ;
#14009 = ORIENTED_EDGE ( 'NONE', *, *, #11948, .F. ) ;
#14010 = ADVANCED_FACE ( 'NONE', ( #16020 ), #3446, .F. ) ;
#14011 = ORIENTED_EDGE ( 'NONE', *, *, #1067, .F. ) ;
#14012 = LINE ( 'NONE', #6715, #14701 ) ;
#14013 = DIRECTION ( 'NONE',  ( -0.000000000000000000, -0.000000000000000000, 1.000000000000000000 ) ) ;
#14014 = VECTOR ( 'NONE', #9119, 1000.000000000000114 ) ;
#14015 = AXIS2_PLACEMENT_3D ( 'NONE', #18078, #9716, #7663 ) ;
#14016 = DIRECTION ( 'NONE',  ( 1.296372316667914327E-16, 1.000000000000000000, -0.000000000000000000 ) ) ;
#14017 = LINE ( 'NONE', #2011, #2134 ) ;
#14018 = CARTESIAN_POINT ( 'NONE',  ( 4.516277899324447453, 39.87315172198108826, 51.91186086883033113 ) ) ;
#14019 = VECTOR ( 'NONE', #215, 1000.000000000000000 ) ;
#14020 = EDGE_CURVE ( 'NONE', #12202, #1817, #8261, .T. ) ;
#14021 = ORIENTED_EDGE ( 'NONE', *, *, #1550, .T. ) ;
#14022 = CARTESIAN_POINT ( 'NONE',  ( 35.00000000000058265, 40.00000000000000000, -55.00000000000076028 ) ) ;
#14023 = CARTESIAN_POINT ( 'NONE',  ( 33.51030287062373247, 15.12081897056669000, -2.800654218530485018 ) ) ;
#14024 = CYLINDRICAL_SURFACE ( 'NONE', #17499, 6.499999999999999112 ) ;
#14025 = DIRECTION ( 'NONE',  ( 0.000000000000000000, -1.000000000000000000, 0.000000000000000000 ) ) ;
#14026 = SURFACE_STYLE_USAGE ( .BOTH. , #5240 ) ;
#14027 = CIRCLE ( 'NONE', #2347, 30.00000000000000000 ) ;
#14028 = DIRECTION ( 'NONE',  ( 6.505213034913038160E-19, 3.903127820947822896E-18, 1.000000000000000000 ) ) ;
#14029 = CIRCLE ( 'NONE', #15501, 34.90673715956759082 ) ;
#14030 = CARTESIAN_POINT ( 'NONE',  ( -6.803227178529575703, 38.81166136533716582, 55.43135129401769490 ) ) ;
#14031 = EDGE_CURVE ( 'NONE', #12228, #22506, #21075, .T. ) ;
#14032 = DIRECTION ( 'NONE',  ( -6.505213034913038160E-19, -3.903127820947822896E-18, -1.000000000000000000 ) ) ;
#14033 = DIRECTION ( 'NONE',  ( -6.505213034913038160E-19, -3.903127820947822896E-18, -1.000000000000000000 ) ) ;
#14034 = VECTOR ( 'NONE', #18335, 1000.000000000000000 ) ;
#14035 = ORIENTED_EDGE ( 'NONE', *, *, #18258, .T. ) ;
#14036 = ORIENTED_EDGE ( 'NONE', *, *, #21253, .T. ) ;
#14037 = ADVANCED_FACE ( 'NONE', ( #6993, #334 ), #5276, .T. ) ;
#14038 = EDGE_CURVE ( 'NONE', #2882, #13818, #16996, .T. ) ;
#14039 = ORIENTED_EDGE ( 'NONE', *, *, #1905, .F. ) ;
#14040 = LINE ( 'NONE', #15773, #1989 ) ;
#14041 = AXIS2_PLACEMENT_3D ( 'NONE', #9291, #16269, #3696 ) ;
#14042 = CYLINDRICAL_SURFACE ( 'NONE', #4694, 9.000000000000003553 ) ;
#14043 = AXIS2_PLACEMENT_3D ( 'NONE', #17974, #2278, #11332 ) ;
#14044 = FACE_BOUND ( 'NONE', #3311, .T. ) ;
#14045 = EDGE_CURVE ( 'NONE', #2875, #4972, #6404, .T. ) ;
#14046 = CARTESIAN_POINT ( 'NONE',  ( -42.50000000000000711, -9.600000000000001421, -47.50000000000000000 ) ) ;
#14047 = CARTESIAN_POINT ( 'NONE',  ( -89.99999999999701572, -5.000000000000000000, -2.500000000000038636 ) ) ;
#14048 = CARTESIAN_POINT ( 'NONE',  ( -14.77818138858748931, 33.48299671873984806, -59.09975138256963589 ) ) ;
#14049 = DIRECTION ( 'NONE',  ( 0.000000000000000000, 0.000000000000000000, -1.000000000000000000 ) ) ;
#14050 = ORIENTED_EDGE ( 'NONE', *, *, #7174, .F. ) ;
#14051 = FACE_OUTER_BOUND ( 'NONE', #7067, .T. ) ;
#14052 = DIRECTION ( 'NONE',  ( -1.224646799147353207E-16, 0.000000000000000000, 1.000000000000000000 ) ) ;
#14053 = EDGE_CURVE ( 'NONE', #6208, #6579, #21414, .T. ) ;
#14054 = DIRECTION ( 'NONE',  ( 0.1421319796954322034, 0.000000000000000000, 0.9898477157360405787 ) ) ;
#14055 = DIRECTION ( 'NONE',  ( 6.505213034913038160E-19, 3.903127820947822896E-18, 1.000000000000000000 ) ) ;
#14056 = EDGE_LOOP ( 'NONE', ( #3800, #7941, #9686, #22037 ) ) ;
#14057 = ADVANCED_FACE ( 'NONE', ( #16248 ), #20044, .T. ) ;
#14058 = AXIS2_PLACEMENT_3D ( 'NONE', #19005, #1128, #13582 ) ;
#14059 = DIRECTION ( 'NONE',  ( -1.000000000000000000, 0.000000000000000000, 0.000000000000000000 ) ) ;
#14060 = LINE ( 'NONE', #19586, #8264 ) ;
#14061 = B_SPLINE_CURVE_WITH_KNOTS ( 'NONE', 1,
 ( #21330, #15930 ),
 .UNSPECIFIED., .F., .F.,
 ( 2, 2 ),
 ( 0.000000000000000000, 1.000000000000000000 ),
 .UNSPECIFIED. ) ;
#14062 = AXIS2_PLACEMENT_3D ( 'NONE', #20840, #3417, #19006 ) ;
#14063 = ORIENTED_EDGE ( 'NONE', *, *, #1917, .F. ) ;
#14064 = VECTOR ( 'NONE', #16480, 1000.000000000000114 ) ;
#14065 = EDGE_CURVE ( 'NONE', #18120, #15589, #3488, .T. ) ;
#14066 = ORIENTED_EDGE ( 'NONE', *, *, #20183, .T. ) ;
#14067 = DIRECTION ( 'NONE',  ( 0.000000000000000000, 0.000000000000000000, 1.000000000000000000 ) ) ;
#14068 = CARTESIAN_POINT ( 'NONE',  ( -34.84300730320195072, 6.953913411054657878, 3.000000000000048850 ) ) ;
#14069 = AXIS2_PLACEMENT_3D ( 'NONE', #3667, #10287, #20963 ) ;
#14070 = DIRECTION ( 'NONE',  ( -0.000000000000000000, -0.000000000000000000, 1.000000000000000000 ) ) ;
#14071 = DIRECTION ( 'NONE',  ( 6.505213034913038160E-19, 3.903127820947822896E-18, 1.000000000000000000 ) ) ;
#14072 = DIRECTION ( 'NONE',  ( 1.000000000000000000, 0.000000000000000000, 0.000000000000000000 ) ) ;
#14073 = ORIENTED_EDGE ( 'NONE', *, *, #11966, .F. ) ;
#14074 = DIRECTION ( 'NONE',  ( -1.000000000000000000, 0.000000000000000000, 0.000000000000000000 ) ) ;
#14075 = DIRECTION ( 'NONE',  ( -6.505213034913038160E-19, -3.903127820947822896E-18, -1.000000000000000000 ) ) ;
#14076 = EDGE_LOOP ( 'NONE', ( #6836, #19270 ) ) ;
#14077 = CYLINDRICAL_SURFACE ( 'NONE', #14877, 2.499999999999998668 ) ;
#14078 = CARTESIAN_POINT ( 'NONE',  ( -6.696867368503558448E-15, 40.00000000000000000, -48.73397172404479960 ) ) ;
#14079 = AXIS2_PLACEMENT_3D ( 'NONE', #18999, #16924, #15528 ) ;
#14080 = DIRECTION ( 'NONE',  ( -0.000000000000000000, 1.000000000000000000, -0.000000000000000000 ) ) ;
#14081 = LINE ( 'NONE', #3245, #16991 ) ;
#14082 = ORIENTED_EDGE ( 'NONE', *, *, #19291, .T. ) ;
#14083 = CARTESIAN_POINT ( 'NONE',  ( -10.00000000000000000, -4.824555320336763486, 3.000000000000000000 ) ) ;
#14084 = CARTESIAN_POINT ( 'NONE',  ( -35.00000000000000000, -9.000000000000001776, -8.999999999999989342 ) ) ;
#14085 = VERTEX_POINT ( 'NONE', #18315 ) ;
#14086 = DIRECTION ( 'NONE',  ( -1.000000000000000000, -1.208970125616081209E-17, 0.000000000000000000 ) ) ;
#14087 = FACE_OUTER_BOUND ( 'NONE', #16517, .T. ) ;
#14088 = CIRCLE ( 'NONE', #7176, 16.49999999999999645 ) ;
#14089 = CIRCLE ( 'NONE', #4633, 3.999999999999999112 ) ;
#14090 = AXIS2_PLACEMENT_3D ( 'NONE', #13445, #1203, #13666 ) ;
#14091 = VECTOR ( 'NONE', #3897, 1000.000000000000000 ) ;
#14092 = EDGE_LOOP ( 'NONE', ( #16301, #745, #3190, #8471 ) ) ;
#14093 = CIRCLE ( 'NONE', #20721, 0.9999999999999974465 ) ;
#14094 = VERTEX_POINT ( 'NONE', #792 ) ;
#14095 = B_SPLINE_CURVE_WITH_KNOTS ( 'NONE', 3,
 ( #11683, #920, #16501, #7915 ),
 .UNSPECIFIED., .F., .F.,
 ( 4, 4 ),
 ( 0.001875451646902739260, 0.003761979286330971450 ),
 .UNSPECIFIED. ) ;
#14096 = VERTEX_POINT ( 'NONE', #17865 ) ;
#14097 = EDGE_CURVE ( 'NONE', #2692, #9285, #10766, .T. ) ;
#14098 = ORIENTED_EDGE ( 'NONE', *, *, #9867, .T. ) ;
#14099 = CARTESIAN_POINT ( 'NONE',  ( -35.00000000000058265, 40.00000000000000000, -55.00000000000076028 ) ) ;
#14100 = DIRECTION ( 'NONE',  ( 0.000000000000000000, 0.000000000000000000, 1.000000000000000000 ) ) ;
#14101 = CYLINDRICAL_SURFACE ( 'NONE', #3707, 1.000000000000000888 ) ;
#14102 = CARTESIAN_POINT ( 'NONE',  ( 5.890136539964617057, 39.99999999999999289, 52.04311943146325348 ) ) ;
#14103 = ORIENTED_EDGE ( 'NONE', *, *, #18365, .F. ) ;
#14104 = FACE_OUTER_BOUND ( 'NONE', #535, .T. ) ;
#14105 = CARTESIAN_POINT ( 'NONE',  ( -1.387778780781445676E-14, 20.00000000000000000, 102.0000000000000142 ) ) ;
#14106 = EDGE_LOOP ( 'NONE', ( #13659, #18166, #21613, #13049 ) ) ;
#14107 = AXIS2_PLACEMENT_3D ( 'NONE', #12303, #14225, #19419 ) ;
#14108 = CARTESIAN_POINT ( 'NONE',  ( -7.544777747232855880, -0.4935208846046454934, 52.99868632946503766 ) ) ;
#14109 = AXIS2_PLACEMENT_3D ( 'NONE', #17652, #5299, #6911 ) ;
#14110 = DIRECTION ( 'NONE',  ( 1.000000000000000000, 0.000000000000000000, 0.000000000000000000 ) ) ;
#14111 = TOROIDAL_SURFACE ( 'NONE', #4265, 34.90673715956759082, 8.750000000000000000 ) ;
#14112 = DIRECTION ( 'NONE',  ( -1.000000000000000000, 1.275531967630005492E-16, 0.000000000000000000 ) ) ;
#14113 = ORIENTED_EDGE ( 'NONE', *, *, #9724, .F. ) ;
#14114 = DIRECTION ( 'NONE',  ( -0.000000000000000000, 1.000000000000000000, -0.000000000000000000 ) ) ;
#14115 = ADVANCED_FACE ( 'NONE', ( #5717 ), #19817, .T. ) ;
#14116 = ORIENTED_EDGE ( 'NONE', *, *, #4356, .F. ) ;
#14117 = CARTESIAN_POINT ( 'NONE',  ( -34.99999999999999289, 5.000000000000000000, 9.000000000000007105 ) ) ;
#14118 = DIRECTION ( 'NONE',  ( 0.000000000000000000, 0.000000000000000000, -1.000000000000000000 ) ) ;
#14119 = CARTESIAN_POINT ( 'NONE',  ( -89.99999999999701572, -5.000000000000000000, 2.499999999999978684 ) ) ;
#14120 = CARTESIAN_POINT ( 'NONE',  ( 15.62751878813134532, 32.48885827236527035, 59.38785559521994628 ) ) ;
#14121 = CYLINDRICAL_SURFACE ( 'NONE', #2675, 31.50000000000000000 ) ;
#14122 = CARTESIAN_POINT ( 'NONE',  ( 2.220446049250313081E-13, 2.775557561562891351E-14, -2.800654218530485018 ) ) ;
#14123 = CIRCLE ( 'NONE', #9023, 58.99999999999994316 ) ;
#14124 = EDGE_LOOP ( 'NONE', ( #15058, #10815, #15463, #14595 ) ) ;
#14125 = ADVANCED_FACE ( 'NONE', ( #439 ), #10985, .T. ) ;
#14126 = EDGE_LOOP ( 'NONE', ( #19325, #1291, #16779, #5074 ) ) ;
#14127 = B_SPLINE_CURVE_WITH_KNOTS ( 'NONE', 3,
 ( #19832, #11108, #12707, #17644, #12476, #21206, #16038, #19601, #7564, #19488, #8938, #14305, #3794, #17987, #17761, #16140, #1953, #14543, #2067, #348, #12928, #7337, #21553, #3911, #10878, #2183, #2870, #1030, #2754, #16723, #8134, #20060, #7911, #18328, #21897, #14985, #9736, #13489, #16842, #9951, #14763 ),
 .UNSPECIFIED., .F., .F.,
 ( 4, 1, 1, 1, 1, 2, 2, 1, 1, 1, 1, 2, 2, 1, 1, 1, 2, 2, 1, 1, 1, 2, 2, 1, 1, 1, 2, 2, 4 ),
 ( 0.000000000000000000, 0.06250000000000066613, 0.09375000000000077716, 0.1093750000000005412, 0.1171875000000003331, 0.1210937500000000278, 0.1249999999999997224, 0.1874999999999943101, 0.2187499999999919509, 0.2343749999999911182, 0.2421874999999908129, 0.2460937499999905353, 0.2499999999999902855, 0.3124999999999911737, 0.3437499999999912292, 0.3593749999999912847, 0.3671874999999913958, 0.3749999999999915623, 0.4374999999999924505, 0.4687499999999932276, 0.4843749999999932832, 0.4921874999999932832, 0.4999999999999933387, 0.6249999999999938938, 0.6874999999999937828, 0.7187499999999942268, 0.7343749999999944489, 0.7499999999999947820, 1.000000000000000000 ),
 .UNSPECIFIED. ) ;
#14128 = EDGE_LOOP ( 'NONE', ( #4904, #4126, #22022, #16169, #2946 ) ) ;
#14129 = ORIENTED_EDGE ( 'NONE', *, *, #11016, .T. ) ;
#14130 = DIRECTION ( 'NONE',  ( -1.000000000000000000, -1.815202222194848473E-15, 0.000000000000000000 ) ) ;
#14131 = CIRCLE ( 'NONE', #13721, 25.00000000000000000 ) ;
#14132 = CARTESIAN_POINT ( 'NONE',  ( -12.31876324338254669, -30.07487443287981677, -6.999999999999950262 ) ) ;
#14133 = CARTESIAN_POINT ( 'NONE',  ( 3.849727973822421485E-15, 1.499999999999997780, 0.000000000000000000 ) ) ;
#14134 = CARTESIAN_POINT ( 'NONE',  ( 24.24871130596423185, 14.00000000000009592, 2.999999999999995559 ) ) ;
#14135 = CARTESIAN_POINT ( 'NONE',  ( 0.03423019660800662167, 39.99999309938340275, 48.76060158720252957 ) ) ;
#14136 = ORIENTED_EDGE ( 'NONE', *, *, #4297, .F. ) ;
#14137 = CARTESIAN_POINT ( 'NONE',  ( -34.99999999999980815, 40.00000000000000711, 57.52499999999922409 ) ) ;
#14138 = VECTOR ( 'NONE', #10312, 1000.000000000000000 ) ;
#14139 = DIRECTION ( 'NONE',  ( -1.000000000000000000, 1.597512185334606831E-14, 0.000000000000000000 ) ) ;
#14140 = DIRECTION ( 'NONE',  ( -0.000000000000000000, 1.000000000000000000, -0.000000000000000000 ) ) ;
#14141 = LINE ( 'NONE', #16212, #580 ) ;
#14142 = VECTOR ( 'NONE', #12796, 1000.000000000000000 ) ;
#14143 = CARTESIAN_POINT ( 'NONE',  ( -7.505578006075234399, 1.461761173328249175, -55.63523492904088386 ) ) ;
#14144 = CARTESIAN_POINT ( 'NONE',  ( -17.21151300967881426, 30.19805602791846155, 59.88250013944312400 ) ) ;
#14145 = EDGE_CURVE ( 'NONE', #13471, #3795, #12804, .T. ) ;
#14146 = FACE_OUTER_BOUND ( 'NONE', #16388, .T. ) ;
#14147 = PRODUCT_RELATED_PRODUCT_CATEGORY ( 'part', '', ( #17518 ) ) ;
#14148 = DIRECTION ( 'NONE',  ( -0.000000000000000000, -1.000000000000000000, -0.000000000000000000 ) ) ;
#14149 = DIRECTION ( 'NONE',  ( -1.000000000000000000, -1.208970125616060717E-17, 0.000000000000000000 ) ) ;
#14150 = CARTESIAN_POINT ( 'NONE',  ( 0.000000000000000000, 30.00000000000000000, 0.000000000000000000 ) ) ;
#14151 = ORIENTED_EDGE ( 'NONE', *, *, #5957, .T. ) ;
#14152 = ADVANCED_FACE ( 'NONE', ( #12690 ), #16593, .F. ) ;
#14153 = VECTOR ( 'NONE', #15125, 1000.000000000000000 ) ;
#14154 = ORIENTED_EDGE ( 'NONE', *, *, #18615, .T. ) ;
#14155 = AXIS2_PLACEMENT_3D ( 'NONE', #15889, #21183, #9146 ) ;
#14156 = AXIS2_PLACEMENT_3D ( 'NONE', #7415, #21064, #5366 ) ;
#14157 = ORIENTED_EDGE ( 'NONE', *, *, #975, .F. ) ;
#14158 = CARTESIAN_POINT ( 'NONE',  ( 7.480086125711145506, -0.2526605362862675563, -53.02285530597580276 ) ) ;
#14159 = DIRECTION ( 'NONE',  ( -6.505213034913038160E-19, -3.903127820947822896E-18, -1.000000000000000000 ) ) ;
#14160 = CARTESIAN_POINT ( 'NONE',  ( -30.00000000000001421, 20.00000000000000355, 105.0000000000000142 ) ) ;
#14161 = ADVANCED_FACE ( 'NONE', ( #4120 ), #4018, .F. ) ;
#14162 = CARTESIAN_POINT ( 'NONE',  ( -34.99999999999999289, 0.000000000000000000, -3.012171160963566127E-14 ) ) ;
#14163 = CARTESIAN_POINT ( 'NONE',  ( 1.110223024625156540E-13, -5.551115123125782702E-14, -6.999999999999950262 ) ) ;
#14164 = CARTESIAN_POINT ( 'NONE',  ( -11.57708680448422101, 39.19108614651867839, -55.24531487870292068 ) ) ;
#14165 = FACE_OUTER_BOUND ( 'NONE', #14106, .T. ) ;
#14166 = VECTOR ( 'NONE', #12237, 1000.000000000000000 ) ;
#14167 = VERTEX_POINT ( 'NONE', #14524 ) ;
#14168 = CYLINDRICAL_SURFACE ( 'NONE', #11954, 19.11328065563152379 ) ;
#14169 = VECTOR ( 'NONE', #8790, 1000.000000000000000 ) ;
#14170 = CARTESIAN_POINT ( 'NONE',  ( 36.75746821813308429, -0.6841746959067585010, 2.800654218530485018 ) ) ;
#14171 = DIRECTION ( 'NONE',  ( 1.000000000000000000, 0.000000000000000000, 0.000000000000000000 ) ) ;
#14172 = DIRECTION ( 'NONE',  ( 0.000000000000000000, 0.000000000000000000, 1.000000000000000000 ) ) ;
#14173 = EDGE_CURVE ( 'NONE', #12233, #11729, #22130, .T. ) ;
#14174 = CARTESIAN_POINT ( 'NONE',  ( -34.99999999999980815, 28.00000000000000000, 52.49999999999922551 ) ) ;
#14175 = AXIS2_PLACEMENT_3D ( 'NONE', #17362, #64, #5129 ) ;
#14176 = ORIENTED_EDGE ( 'NONE', *, *, #11051, .T. ) ;
#14177 = CARTESIAN_POINT ( 'NONE',  ( 5.551115123125782702E-14, -1.387778780781445676E-13, -5.749999999999949374 ) ) ;
#14178 = DIRECTION ( 'NONE',  ( 6.505213034913038160E-19, 3.903127820947822896E-18, 1.000000000000000000 ) ) ;
#14179 = ORIENTED_EDGE ( 'NONE', *, *, #2232, .T. ) ;
#14180 = CIRCLE ( 'NONE', #4342, 9.000000000000003553 ) ;
#14181 = CIRCLE ( 'NONE', #22278, 41.00000000000000000 ) ;
#14182 = AXIS2_PLACEMENT_3D ( 'NONE', #6363, #6479, #10017 ) ;
#14183 = CIRCLE ( 'NONE', #20461, 1.000000000000001776 ) ;
#14184 = VERTEX_POINT ( 'NONE', #21881 ) ;
#14185 = CARTESIAN_POINT ( 'NONE',  ( 1.572625745562107991, 24.67014512736552945, 6.879522542764194171 ) ) ;
#14186 = CARTESIAN_POINT ( 'NONE',  ( 2.220446049250313081E-13, 2.775557561562891351E-14, -2.800654218530485018 ) ) ;
#14187 = DIRECTION ( 'NONE',  ( -6.505213034913038160E-19, -3.903127820947822896E-18, -1.000000000000000000 ) ) ;
#14188 = EDGE_CURVE ( 'NONE', #651, #21559, #14641, .T. ) ;
#14189 = CARTESIAN_POINT ( 'NONE',  ( 35.00000000000000000, -4.999999999999997335, 57.00000000000002842 ) ) ;
#14190 = VERTEX_POINT ( 'NONE', #6179 ) ;
#14191 = CARTESIAN_POINT ( 'NONE',  ( 11.85401191286899980, 32.83234229683715455, 2.999999999999995559 ) ) ;
#14192 = DIRECTION ( 'NONE',  ( 0.000000000000000000, 1.000000000000000000, -0.000000000000000000 ) ) ;
#14193 = ORIENTED_EDGE ( 'NONE', *, *, #10107, .T. ) ;
#14194 = DIRECTION ( 'NONE',  ( -6.505213034913038160E-19, -3.903127820947822896E-18, -1.000000000000000000 ) ) ;
#14195 = DIRECTION ( 'NONE',  ( -1.000000000000000000, 1.264902534566437453E-16, 0.000000000000000000 ) ) ;
#14196 = DIRECTION ( 'NONE',  ( 0.000000000000000000, 0.000000000000000000, -1.000000000000000000 ) ) ;
#14197 = VECTOR ( 'NONE', #14423, 1000.000000000000000 ) ;
#14198 = ORIENTED_EDGE ( 'NONE', *, *, #5126, .T. ) ;
#14199 = DIRECTION ( 'NONE',  ( -0.000000000000000000, 1.000000000000000000, -0.000000000000000000 ) ) ;
#14200 = CARTESIAN_POINT ( 'NONE',  ( -8.923978417721194489, 2.083761144194138826, 56.51262908348098790 ) ) ;
#14201 = CIRCLE ( 'NONE', #3776, 3.000000000000002665 ) ;
#14202 = EDGE_CURVE ( 'NONE', #4210, #20847, #17371, .T. ) ;
#14203 = EDGE_CURVE ( 'NONE', #21010, #10333, #9605, .T. ) ;
#14204 = CARTESIAN_POINT ( 'NONE',  ( -1.107481333971237270, 39.99270069144557027, -49.57628751188472194 ) ) ;
#14205 = EDGE_CURVE ( 'NONE', #10374, #17205, #13693, .T. ) ;
#14206 = ORIENTED_EDGE ( 'NONE', *, *, #7313, .F. ) ;
#14207 = DIRECTION ( 'NONE',  ( -0.000000000000000000, -1.000000000000000000, -0.000000000000000000 ) ) ;
#14208 = LINE ( 'NONE', #21444, #15469 ) ;
#14209 = AXIS2_PLACEMENT_3D ( 'NONE', #1053, #20189, #21677 ) ;
#14210 = EDGE_CURVE ( 'NONE', #15828, #9080, #18475, .T. ) ;
#14211 = ORIENTED_EDGE ( 'NONE', *, *, #9526, .F. ) ;
#14212 = ORIENTED_EDGE ( 'NONE', *, *, #9608, .F. ) ;
#14213 = AXIS2_PLACEMENT_3D ( 'NONE', #14941, #7856, #6481 ) ;
#14214 = VERTEX_POINT ( 'NONE', #18885 ) ;
#14215 = ORIENTED_EDGE ( 'NONE', *, *, #19563, .T. ) ;
#14216 = DIRECTION ( 'NONE',  ( 0.000000000000000000, 0.000000000000000000, 1.000000000000000000 ) ) ;
#14217 = DIRECTION ( 'NONE',  ( 0.000000000000000000, 0.000000000000000000, -1.000000000000000000 ) ) ;
#14218 = CARTESIAN_POINT ( 'NONE',  ( 8.774784205810801652, 39.47271969504190281, -54.19450391025852554 ) ) ;
#14219 = DIRECTION ( 'NONE',  ( -6.505213034913038160E-19, -3.903127820947822896E-18, -1.000000000000000000 ) ) ;
#14220 = ORIENTED_EDGE ( 'NONE', *, *, #18515, .T. ) ;
#14221 = DIRECTION ( 'NONE',  ( -1.000000000000000000, -4.356485333267636965E-15, 0.000000000000000000 ) ) ;
#14222 = DIRECTION ( 'NONE',  ( 6.505213034913038160E-19, 3.903127820947822896E-18, 1.000000000000000000 ) ) ;
#14223 = EDGE_LOOP ( 'NONE', ( #14325, #14968, #15563 ) ) ;
#14224 = CARTESIAN_POINT ( 'NONE',  ( 20.36304159388371815, 24.03323817228478276, -2.999999999999999112 ) ) ;
#14225 = DIRECTION ( 'NONE',  ( -6.505213034913038160E-19, -3.903127820947822896E-18, -1.000000000000000000 ) ) ;
#14226 = CARTESIAN_POINT ( 'NONE',  ( 34.99999999999980815, 40.00000000000000711, 57.52499999999922409 ) ) ;
#14227 = VERTEX_POINT ( 'NONE', #6512 ) ;
#14228 = LINE ( 'NONE', #8865, #667 ) ;
#14229 = VERTEX_POINT ( 'NONE', #1129 ) ;
#14230 = CARTESIAN_POINT ( 'NONE',  ( -9.999999999999758415, -3.000000000000169198, -4.999999999999984013 ) ) ;
#14231 = DIRECTION ( 'NONE',  ( 6.505213034913038160E-19, 3.903127820947822896E-18, 1.000000000000000000 ) ) ;
#14232 = CARTESIAN_POINT ( 'NONE',  ( -8.485281374238429208, 2.999999999999808153, 5.000000000000018652 ) ) ;
#14233 = DIRECTION ( 'NONE',  ( -0.000000000000000000, -1.000000000000000000, -0.000000000000000000 ) ) ;
#14234 = DIRECTION ( 'NONE',  ( 0.000000000000000000, 0.000000000000000000, 1.000000000000000000 ) ) ;
#14235 = AXIS2_PLACEMENT_3D ( 'NONE', #4113, #11084, #2391 ) ;
#14236 = CARTESIAN_POINT ( 'NONE',  ( 19.97206123483663731, 21.14267036293957247, 58.14006880918460496 ) ) ;
#14237 = DIRECTION ( 'NONE',  ( 0.000000000000000000, 0.7071067811866457165, 0.7071067811864494290 ) ) ;
#14238 = ADVANCED_FACE ( 'NONE', ( #3193 ), #15422, .F. ) ;
#14239 = EDGE_CURVE ( 'NONE', #21378, #2694, #8589, .T. ) ;
#14240 = CARTESIAN_POINT ( 'NONE',  ( 28.14364593009904425, -21.69710536060321715, 3.000000000000048850 ) ) ;
#14241 = ORIENTED_EDGE ( 'NONE', *, *, #4469, .T. ) ;
#14242 = AXIS2_PLACEMENT_3D ( 'NONE', #226, #14070, #17876 ) ;
#14243 = ORIENTED_EDGE ( 'NONE', *, *, #11800, .T. ) ;
#14244 = ADVANCED_FACE ( 'NONE', ( #15080 ), #13477, .F. ) ;
#14245 = VERTEX_POINT ( 'NONE', #4907 ) ;
#14246 = ORIENTED_EDGE ( 'NONE', *, *, #13798, .T. ) ;
#14247 = CARTESIAN_POINT ( 'NONE',  ( -24.79619811426189813, 21.00948735876859175, -2.999999999999999112 ) ) ;
#14248 = DIRECTION ( 'NONE',  ( -0.000000000000000000, -0.000000000000000000, 1.000000000000000000 ) ) ;
#14249 = DIRECTION ( 'NONE',  ( -1.000000000000000000, 0.000000000000000000, 1.445602896647339163E-16 ) ) ;
#14250 = ADVANCED_BREP_SHAPE_REPRESENTATION ( '', ( #17752, #18273 ), #17150 ) ;
#14251 = AXIS2_PLACEMENT_3D ( 'NONE', #3754, #10711, #17716 ) ;
#14252 = CYLINDRICAL_SURFACE ( 'NONE', #8736, 1.000000000000000888 ) ;
#14253 = LINE ( 'NONE', #4161, #22283 ) ;
#14254 = CARTESIAN_POINT ( 'NONE',  ( 4.556497390243006151, 39.87079205654652725, 51.93698194406282198 ) ) ;
#14255 = ORIENTED_EDGE ( 'NONE', *, *, #397, .T. ) ;
#14256 = DIRECTION ( 'NONE',  ( 0.000000000000000000, 0.7071067811865474617, 0.7071067811865474617 ) ) ;
#14257 = CARTESIAN_POINT ( 'NONE',  ( 7.463862311151453710, 35.99819890246955367, 2.800654218530485018 ) ) ;
#14258 = CYLINDRICAL_SURFACE ( 'NONE', #7626, 2.099999999999997868 ) ;
#14259 = CARTESIAN_POINT ( 'NONE',  ( -5.833333333333325932, 40.00000000000000000, 40.61164310337068883 ) ) ;
#14260 = CARTESIAN_POINT ( 'NONE',  ( -10.99584631063759588, 3.272668205460579127, -57.61971594758655613 ) ) ;
#14261 = APPLICATION_CONTEXT ( 'automotive_design' ) ;
#14262 = EDGE_CURVE ( 'NONE', #22326, #19879, #10038, .T. ) ;
#14263 = AXIS2_PLACEMENT_3D ( 'NONE', #8191, #22177, #1096 ) ;
#14264 = DIRECTION ( 'NONE',  ( -0.000000000000000000, -1.000000000000000000, -0.000000000000000000 ) ) ;
#14265 = DIRECTION ( 'NONE',  ( -0.000000000000000000, -1.000000000000000000, -0.000000000000000000 ) ) ;
#14266 = DIRECTION ( 'NONE',  ( 1.000000000000000000, 0.000000000000000000, -1.224646799147353207E-16 ) ) ;
#14267 = VERTEX_POINT ( 'NONE', #1016 ) ;
#14268 = EDGE_LOOP ( 'NONE', ( #4803, #17475, #2770, #22059 ) ) ;
#14269 = ORIENTED_EDGE ( 'NONE', *, *, #19340, .T. ) ;
#14270 = CARTESIAN_POINT ( 'NONE',  ( -6.953913411054715610, -34.84300730320209283, 3.000000000000044409 ) ) ;
#14271 = AXIS2_PLACEMENT_3D ( 'NONE', #15010, #5983, #11364 ) ;
#14272 = DIRECTION ( 'NONE',  ( 1.000000000000000000, 1.208970125616063182E-17, 0.000000000000000000 ) ) ;
#14273 = ADVANCED_FACE ( 'NONE', ( #4798 ), #10159, .F. ) ;
#14274 = LINE ( 'NONE', #14937, #5153 ) ;
#14275 = DIRECTION ( 'NONE',  ( 6.505213034913038160E-19, 3.903127820947822896E-18, 1.000000000000000000 ) ) ;
#14276 = EDGE_CURVE ( 'NONE', #16403, #20378, #22100, .T. ) ;
#14277 = CARTESIAN_POINT ( 'NONE',  ( -14.84934717125631920, 6.596698521592471387, 59.12425370493867405 ) ) ;
#14278 = DIRECTION ( 'NONE',  ( 0.000000000000000000, -0.7071067811865500152, -0.7071067811865451302 ) ) ;
#14279 = CARTESIAN_POINT ( 'NONE',  ( 0.000000000000000000, 7.000000000000000000, 0.000000000000000000 ) ) ;
#14280 = ADVANCED_FACE ( 'NONE', ( #20385 ), #17153, .T. ) ;
#14281 = EDGE_CURVE ( 'NONE', #3949, #21644, #18841, .T. ) ;
#14282 = VERTEX_POINT ( 'NONE', #9842 ) ;
#14283 = DIRECTION ( 'NONE',  ( -1.000000000000000000, -1.208970125616046080E-17, 6.505213034913038160E-19 ) ) ;
#14284 = LINE ( 'NONE', #12682, #3423 ) ;
#14285 = DIRECTION ( 'NONE',  ( 1.000000000000000000, 0.000000000000000000, 0.000000000000000000 ) ) ;
#14286 = LINE ( 'NONE', #21530, #14064 ) ;
#14287 = CARTESIAN_POINT ( 'NONE',  ( 25.00000000000000000, 20.00000000000000000, -16.49999999999997868 ) ) ;
#14288 = ORIENTED_EDGE ( 'NONE', *, *, #22531, .F. ) ;
#14289 = AXIS2_PLACEMENT_3D ( 'NONE', #8266, #22600, #20531 ) ;
#14290 = B_SPLINE_CURVE_WITH_KNOTS ( 'NONE', 3,
 ( #271, #1999, #5142, #2226 ),
 .UNSPECIFIED., .F., .F.,
 ( 4, 4 ),
 ( 9.715086410652220024E-07, 0.001929643240672559339 ),
 .UNSPECIFIED. ) ;
#14291 = CARTESIAN_POINT ( 'NONE',  ( 24.75236754129178607, 27.84804035626031649, -2.999999999999971578 ) ) ;
#14292 = DIRECTION ( 'NONE',  ( 0.000000000000000000, 0.000000000000000000, 1.000000000000000000 ) ) ;
#14293 = CARTESIAN_POINT ( 'NONE',  ( 16.25447798254043263, 8.309829536807932016, -57.03340146943282463 ) ) ;
#14294 = EDGE_CURVE ( 'NONE', #15936, #15170, #13583, .T. ) ;
#14295 = ORIENTED_EDGE ( 'NONE', *, *, #4056, .F. ) ;
#14296 = VECTOR ( 'NONE', #13855, 1000.000000000000000 ) ;
#14297 = CIRCLE ( 'NONE', #10633, 9.000000000000003553 ) ;
#14298 = ADVANCED_FACE ( 'NONE', ( #6398 ), #20596, .F. ) ;
#14299 = ORIENTED_EDGE ( 'NONE', *, *, #12132, .T. ) ;
#14300 = CARTESIAN_POINT ( 'NONE',  ( 2.670518050928090137, 23.57199239071502817, 6.613211112165401140 ) ) ;
#14301 = CARTESIAN_POINT ( 'NONE',  ( 25.00000000000000355, 20.00000000000000000, 25.00000000000000711 ) ) ;
#14302 = LINE ( 'NONE', #110, #2149 ) ;
#14303 = VERTEX_POINT ( 'NONE', #18664 ) ;
#14304 = CARTESIAN_POINT ( 'NONE',  ( 35.00000000000001421, 0.000000000000000000, -58.99999999999702993 ) ) ;
#14305 = CARTESIAN_POINT ( 'NONE',  ( -7.725157334975624401, 39.99999999999999289, 52.85293811915976647 ) ) ;
#14306 = ORIENTED_EDGE ( 'NONE', *, *, #17750, .T. ) ;
#14307 = CARTESIAN_POINT ( 'NONE',  ( 10.70799354677381920, -35.16985127952404611, -2.800654218530477912 ) ) ;
#14308 = DIRECTION ( 'NONE',  ( -0.000000000000000000, 1.000000000000000000, -0.000000000000000000 ) ) ;
#14309 = CARTESIAN_POINT ( 'NONE',  ( 19.23435001722034698, 8.416038526954860544, -57.89219688981297907 ) ) ;
#14310 = B_SPLINE_CURVE_WITH_KNOTS ( 'NONE', 3,
 ( #6058, #1130, #4578, #13026 ),
 .UNSPECIFIED., .F., .F.,
 ( 4, 4 ),
 ( 9.715086410669694314E-07, 0.001929643240672542425 ),
 .UNSPECIFIED. ) ;
#14311 = EDGE_CURVE ( 'NONE', #22510, #21245, #3844, .T. ) ;
#14312 = CARTESIAN_POINT ( 'NONE',  ( -34.99999999999999289, -5.000000000000000000, -3.012171160963566127E-14 ) ) ;
#14313 = ORIENTED_EDGE ( 'NONE', *, *, #22285, .T. ) ;
#14314 = LINE ( 'NONE', #122, #7943 ) ;
#14315 = CARTESIAN_POINT ( 'NONE',  ( 1.734723475976807094E-14, 20.00000000000000000, 20.71067811865476216 ) ) ;
#14316 = CARTESIAN_POINT ( 'NONE',  ( -0.9607552338323060992, 39.99453550393771906, -49.46704700291807910 ) ) ;
#14317 = ORIENTED_EDGE ( 'NONE', *, *, #20358, .T. ) ;
#14318 = CYLINDRICAL_SURFACE ( 'NONE', #21520, 30.00000000000000000 ) ;
#14319 = CIRCLE ( 'NONE', #4468, 1.000000000000000888 ) ;
#14320 = DIRECTION ( 'NONE',  ( 0.000000000000000000, -1.000000000000000000, 0.000000000000000000 ) ) ;
#14321 = DIRECTION ( 'NONE',  ( 0.000000000000000000, 0.000000000000000000, -1.000000000000000000 ) ) ;
#14322 = EDGE_CURVE ( 'NONE', #17708, #12273, #22514, .T. ) ;
#14323 = EDGE_LOOP ( 'NONE', ( #18073, #7335, #21859, #15759 ) ) ;
#14324 = ORIENTED_EDGE ( 'NONE', *, *, #21627, .T. ) ;
#14325 = ORIENTED_EDGE ( 'NONE', *, *, #18498, .F. ) ;
#14326 =( NAMED_UNIT ( * ) PLANE_ANGLE_UNIT ( ) SI_UNIT ( $, .RADIAN. ) );
#14327 = ADVANCED_FACE ( 'NONE', ( #19113 ), #12224, .F. ) ;
#14328 = ORIENTED_EDGE ( 'NONE', *, *, #14532, .T. ) ;
#14329 = DIRECTION ( 'NONE',  ( 6.505213034913038160E-19, 3.903127820947822896E-18, 1.000000000000000000 ) ) ;
#14330 = DIRECTION ( 'NONE',  ( -6.505213034913038160E-19, -3.903127820947822896E-18, -1.000000000000000000 ) ) ;
#14331 = AXIS2_PLACEMENT_3D ( 'NONE', #18680, #9623, #20401 ) ;
#14332 = CARTESIAN_POINT ( 'NONE',  ( 7.259797106483209639, 39.65417185066220895, -53.48039442441829294 ) ) ;
#14333 = CARTESIAN_POINT ( 'NONE',  ( 7.248955570856898234, 40.00000000000000000, 52.65401626641859423 ) ) ;
#14334 = ORIENTED_EDGE ( 'NONE', *, *, #540, .F. ) ;
#14335 = DIRECTION ( 'NONE',  ( -1.000000000000000000, -1.208970125616027129E-17, 0.000000000000000000 ) ) ;
#14336 = CYLINDRICAL_SURFACE ( 'NONE', #3211, 0.9999999999999974465 ) ;
#14337 = ORIENTED_EDGE ( 'NONE', *, *, #9164, .T. ) ;
#14338 = DIRECTION ( 'NONE',  ( -6.505213034913038160E-19, -3.903127820947822896E-18, -1.000000000000000000 ) ) ;
#14339 = CARTESIAN_POINT ( 'NONE',  ( 1.607210943102148261E-12, -4.184048734395063640, 46.01969553071018026 ) ) ;
#14340 = CARTESIAN_POINT ( 'NONE',  ( -42.50000000000000711, -12.00000000000000000, 47.50000000000000711 ) ) ;
#14341 = ORIENTED_EDGE ( 'NONE', *, *, #14554, .T. ) ;
#14342 = CARTESIAN_POINT ( 'NONE',  ( -0.05288783471921253143, -1.234056376215194817, 48.20419181041120993 ) ) ;
#14343 = VERTEX_POINT ( 'NONE', #15872 ) ;
#14344 = DIRECTION ( 'NONE',  ( -0.7071067811865524577, -1.130863789078082253E-17, -0.7071067811865426878 ) ) ;
#14345 = ADVANCED_FACE ( 'NONE', ( #13823 ), #20318, .T. ) ;
#14346 = CARTESIAN_POINT ( 'NONE',  ( -5.666031183648452263, 39.18449859167989757, 54.55698311759263675 ) ) ;
#14347 = CARTESIAN_POINT ( 'NONE',  ( -28.88846368933341324, -19.59430950039325836, -2.999999999999947153 ) ) ;
#14348 = ORIENTED_EDGE ( 'NONE', *, *, #2125, .F. ) ;
#14349 = CARTESIAN_POINT ( 'NONE',  ( 20.11656324090261450, 10.00164725896550522, 58.12608834080169373 ) ) ;
#14350 = CARTESIAN_POINT ( 'NONE',  ( 7.088850870549147224E-15, -5.000000000000000000, 44.98888751680801334 ) ) ;
#14351 = ADVANCED_FACE ( 'NONE', ( #3539 ), #17730, .F. ) ;
#14352 = AXIS2_PLACEMENT_3D ( 'NONE', #9616, #7910, #13156 ) ;
#14353 = FACE_OUTER_BOUND ( 'NONE', #19099, .T. ) ;
#14354 = EDGE_CURVE ( 'NONE', #9080, #15828, #4935, .T. ) ;
#14355 = B_SPLINE_CURVE_WITH_KNOTS ( 'NONE', 3,
 ( #10199, #6321, #3005, #4735 ),
 .UNSPECIFIED., .F., .F.,
 ( 4, 4 ),
 ( 9.715086409635437439E-07, 0.001929643240672442245 ),
 .UNSPECIFIED. ) ;
#14356 = CONICAL_SURFACE ( 'NONE', #11074, 20.00000000000002132, 0.7853981633974543852 ) ;
#14357 = ORIENTED_EDGE ( 'NONE', *, *, #6390, .F. ) ;
#14358 = ORIENTED_EDGE ( 'NONE', *, *, #17374, .F. ) ;
#14359 = ORIENTED_EDGE ( 'NONE', *, *, #10148, .T. ) ;
#14360 = ORIENTED_EDGE ( 'NONE', *, *, #7017, .T. ) ;
#14361 = CARTESIAN_POINT ( 'NONE',  ( -32.10132595304119008, -5.074925817841968723, -2.999999999999971578 ) ) ;
#14362 = CARTESIAN_POINT ( 'NONE',  ( 89.99999999999701572, -5.000000000000000000, -5.216535399428728743E-14 ) ) ;
#14363 = CARTESIAN_POINT ( 'NONE',  ( 25.00000000000000000, 20.00000000000000000, 6.487780019669002523E-15 ) ) ;
#14364 = ORIENTED_EDGE ( 'NONE', *, *, #2621, .F. ) ;
#14365 = FACE_OUTER_BOUND ( 'NONE', #15207, .T. ) ;
#14366 = CARTESIAN_POINT ( 'NONE',  ( 2.220446049250313081E-13, -8.326672684688674053E-14, 2.800654218530498785 ) ) ;
#14367 = B_SPLINE_CURVE_WITH_KNOTS ( 'NONE', 3,
 ( #14694, #11264, #22044, #2796, #6338, #20212 ),
 .UNSPECIFIED., .F., .F.,
 ( 4, 2, 4 ),
 ( 4.605519509344441270E-20, 0.005389490931282739546, 0.01077898186256547909 ),
 .UNSPECIFIED. ) ;
#14368 = EDGE_CURVE ( 'NONE', #12073, #12156, #7861, .T. ) ;
#14369 = ADVANCED_FACE ( 'NONE', ( #10606, #22564, #15767 ), #15658, .T. ) ;
#14370 = AXIS2_PLACEMENT_3D ( 'NONE', #19438, #10480, #3293 ) ;
#14371 = ORIENTED_EDGE ( 'NONE', *, *, #19990, .T. ) ;
#14372 = CARTESIAN_POINT ( 'NONE',  ( 2.220446049250313081E-13, 2.775557561562891351E-14, -2.800654218530485018 ) ) ;
#14373 = AXIS2_PLACEMENT_3D ( 'NONE', #21186, #5488, #5710 ) ;
#14374 = CARTESIAN_POINT ( 'NONE',  ( 6.000000000000000000, -20.00000000000000000, 5.999999999999998224 ) ) ;
#14375 = DIRECTION ( 'NONE',  ( -0.000000000000000000, -1.000000000000000000, -0.000000000000000000 ) ) ;
#14376 = FACE_OUTER_BOUND ( 'NONE', #7931, .T. ) ;
#14377 = EDGE_CURVE ( 'NONE', #11652, #10901, #10274, .T. ) ;
#14378 = CARTESIAN_POINT ( 'NONE',  ( 28.13960001536971234, -21.69517388068267039, -2.999999999999977796 ) ) ;
#14379 = CARTESIAN_POINT ( 'NONE',  ( 4.928914132345181612E-15, 0.000000000000000000, -19.00000000000000355 ) ) ;
#14380 = CARTESIAN_POINT ( 'NONE',  ( 42.50000000000000711, -5.000000000000000000, -47.50000000000000000 ) ) ;
#14381 = ORIENTED_EDGE ( 'NONE', *, *, #10991, .T. ) ;
#14382 = ORIENTED_EDGE ( 'NONE', *, *, #18549, .T. ) ;
#14383 = CIRCLE ( 'NONE', #3441, 9.000000000000035527 ) ;
#14384 = CIRCLE ( 'NONE', #19536, 19.11328065563151668 ) ;
#14385 = ORIENTED_EDGE ( 'NONE', *, *, #4440, .F. ) ;
#14386 = CARTESIAN_POINT ( 'NONE',  ( -42.50000000000000711, -5.000000000000000000, -41.00000000000000000 ) ) ;
#14387 = FACE_OUTER_BOUND ( 'NONE', #7469, .T. ) ;
#14388 = EDGE_CURVE ( 'NONE', #18499, #5003, #20334, .T. ) ;
#14389 = DIRECTION ( 'NONE',  ( -1.000000000000000000, -1.208970125616046080E-17, 6.505213034913038160E-19 ) ) ;
#14390 = CIRCLE ( 'NONE', #7872, 50.00000000000000000 ) ;
#14391 = DIRECTION ( 'NONE',  ( 6.505213034913038160E-19, 3.903127820947822896E-18, 1.000000000000000000 ) ) ;
#14392 = CARTESIAN_POINT ( 'NONE',  ( 41.39271818392636959, 10.00000000000000000, -5.943569790512535533 ) ) ;
#14393 = CARTESIAN_POINT ( 'NONE',  ( 1.423424233832626395, 32.35999952201593288, -6.999999999999999112 ) ) ;
#14394 = CYLINDRICAL_SURFACE ( 'NONE', #2155, 1.000000000000000888 ) ;
#14395 = DIRECTION ( 'NONE',  ( 1.000000000000000000, 0.000000000000000000, 0.000000000000000000 ) ) ;
#14396 = PRODUCT_DEFINITION_SHAPE ( 'NONE', 'NONE',  #306 ) ;
#14397 = ORIENTED_EDGE ( 'NONE', *, *, #2047, .T. ) ;
#14398 = CARTESIAN_POINT ( 'NONE',  ( 42.49999999999998579, 10.00000000000000000, -47.49999999999997868 ) ) ;
#14399 = EDGE_CURVE ( 'NONE', #19879, #16727, #1669, .T. ) ;
#14400 = CARTESIAN_POINT ( 'NONE',  ( 4.000000000000003553, -1.500000000000015543, 4.898587196589412829E-16 ) ) ;
#14401 = DIRECTION ( 'NONE',  ( 0.000000000000000000, 1.000000000000000000, 0.000000000000000000 ) ) ;
#14402 = DIRECTION ( 'NONE',  ( -1.000000000000000000, -2.677423277737400817E-15, 0.000000000000000000 ) ) ;
#14403 = DIRECTION ( 'NONE',  ( 1.000000000000000000, 0.000000000000000000, 0.000000000000000000 ) ) ;
#14404 = CIRCLE ( 'NONE', #21028, 2.099999999999990763 ) ;
#14405 = ORIENTED_EDGE ( 'NONE', *, *, #11267, .T. ) ;
#14406 = LINE ( 'NONE', #4014, #6165 ) ;
#14407 = CARTESIAN_POINT ( 'NONE',  ( -20.00000000000001421, 20.00000000000000000, 60.00200000000000244 ) ) ;
#14408 = DIRECTION ( 'NONE',  ( -0.000000000000000000, -1.000000000000000000, -0.000000000000000000 ) ) ;
#14409 = B_SPLINE_CURVE_WITH_KNOTS ( 'NONE', 1,
 ( #17770, #15924 ),
 .UNSPECIFIED., .F., .F.,
 ( 2, 2 ),
 ( 0.000000000000000000, 1.000000000000000000 ),
 .UNSPECIFIED. ) ;
#14410 = EDGE_CURVE ( 'NONE', #10013, #21090, #16659, .T. ) ;
#14411 = LINE ( 'NONE', #5720, #6382 ) ;
#14412 = ORIENTED_EDGE ( 'NONE', *, *, #18071, .F. ) ;
#14413 = CARTESIAN_POINT ( 'NONE',  ( -10.00000000000000888, 2.999999999999836131, -4.999999999999948486 ) ) ;
#14414 = EDGE_CURVE ( 'NONE', #7816, #6097, #927, .T. ) ;
#14415 = AXIS2_PLACEMENT_3D ( 'NONE', #13871, #5190, #12167 ) ;
#14416 = VERTEX_POINT ( 'NONE', #3653 ) ;
#14417 = DIRECTION ( 'NONE',  ( 0.000000000000000000, 0.000000000000000000, -1.000000000000000000 ) ) ;
#14418 = CARTESIAN_POINT ( 'NONE',  ( -12.09218358684865002, 1.291952833854525196, 55.42846997241219498 ) ) ;
#14419 = ORIENTED_EDGE ( 'NONE', *, *, #930, .T. ) ;
#14420 = CARTESIAN_POINT ( 'NONE',  ( 34.99999999999980815, 28.00000000000000000, 57.09999999999921982 ) ) ;
#14421 = CARTESIAN_POINT ( 'NONE',  ( -10.62139969368320891, 0.6004703193304483655, -54.70636795414683462 ) ) ;
#14422 = ORIENTED_EDGE ( 'NONE', *, *, #15688, .F. ) ;
#14423 = DIRECTION ( 'NONE',  ( 1.445602896647339163E-16, 0.000000000000000000, 1.000000000000000000 ) ) ;
#14424 = CARTESIAN_POINT ( 'NONE',  ( 23.49999999999998579, 19.99999999999999645, -105.0000000000000142 ) ) ;
#14425 = CARTESIAN_POINT ( 'NONE',  ( 35.00000000000000000, 40.00000000000000000, -59.99999999999999289 ) ) ;
#14426 = FACE_OUTER_BOUND ( 'NONE', #15876, .T. ) ;
#14427 = ORIENTED_EDGE ( 'NONE', *, *, #14483, .T. ) ;
#14428 = DIRECTION ( 'NONE',  ( 0.000000000000000000, 0.000000000000000000, 1.000000000000000000 ) ) ;
#14429 = CIRCLE ( 'NONE', #14058, 2.999999999999999112 ) ;
#14430 = CARTESIAN_POINT ( 'NONE',  ( -8.349099696861312481, 1.803277857259544925, 53.93591755799873511 ) ) ;
#14431 = CARTESIAN_POINT ( 'NONE',  ( -1.076297586510878146, 39.99310908795442288, -49.55312039312080685 ) ) ;
#14432 = AXIS2_PLACEMENT_3D ( 'NONE', #11882, #2969, #8896 ) ;
#14433 = ORIENTED_EDGE ( 'NONE', *, *, #16022, .F. ) ;
#14434 = PLANE ( 'NONE',  #10438 ) ;
#14435 = FACE_OUTER_BOUND ( 'NONE', #16888, .T. ) ;
#14436 = EDGE_CURVE ( 'NONE', #6859, #2966, #20187, .T. ) ;
#14437 = AXIS2_PLACEMENT_3D ( 'NONE', #11501, #16430, #743 ) ;
#14438 = ORIENTED_EDGE ( 'NONE', *, *, #13705, .T. ) ;
#14439 = AXIS2_PLACEMENT_3D ( 'NONE', #18784, #9856, #1034 ) ;
#14440 = EDGE_LOOP ( 'NONE', ( #7087, #14215, #749, #1602 ) ) ;
#14441 = ORIENTED_EDGE ( 'NONE', *, *, #4842, .F. ) ;
#14442 = VERTEX_POINT ( 'NONE', #17609 ) ;
#14443 = DIRECTION ( 'NONE',  ( 1.000000000000000000, 0.000000000000000000, 0.000000000000000000 ) ) ;
#14444 = AXIS2_PLACEMENT_3D ( 'NONE', #3014, #8165, #9982 ) ;
#14445 = DIRECTION ( 'NONE',  ( 1.296372316667914327E-16, 1.000000000000000000, -0.000000000000000000 ) ) ;
#14446 = CARTESIAN_POINT ( 'NONE',  ( 35.00000000000001421, 0.000000000000000000, 1.540743955509788682E-30 ) ) ;
#14447 = CARTESIAN_POINT ( 'NONE',  ( 17.09029715894935819, -27.64365646977296009, 2.999999999999995559 ) ) ;
#14448 = ORIENTED_EDGE ( 'NONE', *, *, #7650, .T. ) ;
#14449 = FACE_OUTER_BOUND ( 'NONE', #21856, .T. ) ;
#14450 = LINE ( 'NONE', #21461, #12701 ) ;
#14451 = ORIENTED_EDGE ( 'NONE', *, *, #9671, .F. ) ;
#14452 = B_SPLINE_CURVE_WITH_KNOTS ( 'NONE', 3,
 ( #8273, #15243, #4621, #9651, #14795, #18471, #22033, #947, #20431, #6327, #21812, #8162, #18706, #2786, #4283, #6444, #831, #19974, #9769, #16758, #4395, #22264, #9979, #18354 ),
 .UNSPECIFIED., .F., .F.,
 ( 4, 2, 2, 2, 2, 2, 2, 2, 2, 2, 2, 4 ),
 ( 0.02614117015034102959, 0.02729036340605314054, 0.02843955666176525149, 0.03073794317318947686, 0.03188713642890158434, 0.03303632968461369529, 0.03533471619603791025, 0.03648390945175002814, 0.03763310270746213909, 0.03993148921888636793, 0.04222987573031060371, 0.04452826224173483255 ),
 .UNSPECIFIED. ) ;
#14453 = FACE_OUTER_BOUND ( 'NONE', #18955, .T. ) ;
#14454 = CARTESIAN_POINT ( 'NONE',  ( -32.14641817400173807, -18.83615802559818064, -6.999999999999992006 ) ) ;
#14455 = DIRECTION ( 'NONE',  ( -0.000000000000000000, -0.000000000000000000, -1.000000000000000000 ) ) ;
#14456 = VERTEX_POINT ( 'NONE', #6818 ) ;
#14457 = ADVANCED_FACE ( 'NONE', ( #13660 ), #17012, .F. ) ;
#14458 = CARTESIAN_POINT ( 'NONE',  ( -5.833333333333339255, 0.000000000000000000, -40.61164310337066041 ) ) ;
#14459 = CARTESIAN_POINT ( 'NONE',  ( 1.427811580246491241, 39.96253266219668632, -50.08434179903181160 ) ) ;
#14460 = VECTOR ( 'NONE', #20552, 1000.000000000000000 ) ;
#14461 = DIRECTION ( 'NONE',  ( 0.000000000000000000, 1.000000000000000000, 0.000000000000000000 ) ) ;
#14462 = CARTESIAN_POINT ( 'NONE',  ( -13.00000000000011546, 42.51666049839536043, 105.0000000000000142 ) ) ;
#14463 = VECTOR ( 'NONE', #11854, 1000.000000000000000 ) ;
#14464 = ORIENTED_EDGE ( 'NONE', *, *, #20210, .T. ) ;
#14465 = CARTESIAN_POINT ( 'NONE',  ( 34.99999999999980815, 40.00000000000000711, 57.52499999999922409 ) ) ;
#14466 = CARTESIAN_POINT ( 'NONE',  ( 19.27384183542241658, 25.35969264784004906, 57.95172789105618705 ) ) ;
#14467 = FACE_OUTER_BOUND ( 'NONE', #14901, .T. ) ;
#14468 = AXIS2_PLACEMENT_3D ( 'NONE', #19865, #3721, #15834 ) ;
#14469 = EDGE_CURVE ( 'NONE', #11481, #8384, #19590, .T. ) ;
#14470 = ADVANCED_FACE ( 'NONE', ( #10238 ), #20796, .T. ) ;
#14471 = CIRCLE ( 'NONE', #17403, 2.500000000000002220 ) ;
#14472 = CARTESIAN_POINT ( 'NONE',  ( 15.21899206303239360, 36.51951236530284461, -56.65045400726858560 ) ) ;
#14473 = ORIENTED_EDGE ( 'NONE', *, *, #18385, .F. ) ;
#14474 = ORIENTED_EDGE ( 'NONE', *, *, #12816, .F. ) ;
#14475 = ORIENTED_EDGE ( 'NONE', *, *, #21082, .F. ) ;
#14476 = CIRCLE ( 'NONE', #15931, 50.00000000000000000 ) ;
#14477 = CIRCLE ( 'NONE', #15191, 34.90673715956759082 ) ;
#14478 = ORIENTED_EDGE ( 'NONE', *, *, #3705, .T. ) ;
#14479 = LINE ( 'NONE', #10694, #1563 ) ;
#14480 = CARTESIAN_POINT ( 'NONE',  ( -11.12045539163121255, 39.12082365984661436, -55.06303111106303305 ) ) ;
#14481 = CONICAL_SURFACE ( 'NONE', #2058, 2.099999999999997868, 1.029744258676653867 ) ;
#14482 = DIRECTION ( 'NONE',  ( 0.000000000000000000, 1.000000000000000000, 0.000000000000000000 ) ) ;
#14483 = EDGE_CURVE ( 'NONE', #12228, #5921, #15258, .T. ) ;
#14484 = VERTEX_POINT ( 'NONE', #8091 ) ;
#14485 = CARTESIAN_POINT ( 'NONE',  ( -10.06223851446356043, 39.28158160658968967, -54.67678195792213813 ) ) ;
#14486 = DIRECTION ( 'NONE',  ( 6.505213034913038160E-19, 3.903127820947822896E-18, 1.000000000000000000 ) ) ;
#14487 = CIRCLE ( 'NONE', #7167, 15.00000000000000000 ) ;
#14488 = EDGE_CURVE ( 'NONE', #18025, #3688, #13707, .T. ) ;
#14489 = ORIENTED_EDGE ( 'NONE', *, *, #14576, .F. ) ;
#14490 = DIRECTION ( 'NONE',  ( -6.505213034913038160E-19, -3.903127820947822896E-18, -1.000000000000000000 ) ) ;
#14491 = CYLINDRICAL_SURFACE ( 'NONE', #1782, 2.500000000000002220 ) ;
#14492 = DIRECTION ( 'NONE',  ( 1.296372316667914327E-16, 1.000000000000000000, -0.000000000000000000 ) ) ;
#14493 = SURFACE_STYLE_USAGE ( .BOTH. , #11295 ) ;
#14494 = DIRECTION ( 'NONE',  ( 1.296372316667914327E-16, 1.000000000000000000, -0.000000000000000000 ) ) ;
#14495 = EDGE_CURVE ( 'NONE', #12869, #3845, #4599, .T. ) ;
#14496 = EDGE_CURVE ( 'NONE', #1823, #3953, #10871, .T. ) ;
#14497 = CIRCLE ( 'NONE', #9011, 34.90673715956759082 ) ;
#14498 = EDGE_CURVE ( 'NONE', #1368, #20409, #2936, .T. ) ;
#14499 = DIRECTION ( 'NONE',  ( 0.000000000000000000, 0.000000000000000000, -1.000000000000000000 ) ) ;
#14500 = CARTESIAN_POINT ( 'NONE',  ( 17.86915608785671949, -27.01645732367855146, -6.999999999999950262 ) ) ;
#14501 = EDGE_CURVE ( 'NONE', #5633, #2840, #14811, .T. ) ;
#14502 = EDGE_LOOP ( 'NONE', ( #4229, #22607, #10610, #4384 ) ) ;
#14503 = CIRCLE ( 'NONE', #12319, 0.9999999999999974465 ) ;
#14504 = ORIENTED_EDGE ( 'NONE', *, *, #7749, .F. ) ;
#14505 = ADVANCED_FACE ( 'NONE', ( #10209, #4744 ), #20433, .F. ) ;
#14506 = ORIENTED_EDGE ( 'NONE', *, *, #11650, .T. ) ;
#14507 = DIRECTION ( 'NONE',  ( 0.000000000000000000, 0.000000000000000000, 1.000000000000000000 ) ) ;
#14508 = CARTESIAN_POINT ( 'NONE',  ( -7.505578006075234399, 1.461761173328249175, -55.63523492904088386 ) ) ;
#14509 = VECTOR ( 'NONE', #21298, 1000.000000000000000 ) ;
#14510 = DIRECTION ( 'NONE',  ( 0.000000000000000000, -0.000000000000000000, -1.000000000000000000 ) ) ;
#14511 = CARTESIAN_POINT ( 'NONE',  ( -42.50000000000000711, -9.600000000000001421, 47.50000000000000711 ) ) ;
#14512 = LINE ( 'NONE', #7420, #1778 ) ;
#14513 = CARTESIAN_POINT ( 'NONE',  ( -9.165377225651191395, 37.79989650906291132, -54.16098472236620864 ) ) ;
#14514 = CARTESIAN_POINT ( 'NONE',  ( -14.74639653023226948, 28.96193690644935259, 2.999999999999995559 ) ) ;
#14515 = DIRECTION ( 'NONE',  ( 6.505213034913038160E-19, 3.903127820947822896E-18, 1.000000000000000000 ) ) ;
#14516 = ORIENTED_EDGE ( 'NONE', *, *, #13798, .F. ) ;
#14517 = LINE ( 'NONE', #21528, #9327 ) ;
#14518 = CARTESIAN_POINT ( 'NONE',  ( 30.60042966911735718, 7.474202570535965151, 2.999999999999995559 ) ) ;
#14519 = CARTESIAN_POINT ( 'NONE',  ( 35.00000000000000000, 14.00000000000000000, 2.365113165210053967E-14 ) ) ;
#14520 = DIRECTION ( 'NONE',  ( -0.000000000000000000, -1.000000000000000000, -0.000000000000000000 ) ) ;
#14521 = ORIENTED_EDGE ( 'NONE', *, *, #21365, .T. ) ;
#14522 = AXIS2_PLACEMENT_3D ( 'NONE', #12740, #14222, #9432 ) ;
#14523 = CARTESIAN_POINT ( 'NONE',  ( -16.06969024216331476, -19.15111107797465451, 2.999999999999995559 ) ) ;
#14524 = CARTESIAN_POINT ( 'NONE',  ( 25.00000000000000355, -20.00000000000000000, 25.00000000000000711 ) ) ;
#14525 = CIRCLE ( 'NONE', #12691, 2.524999999999999467 ) ;
#14526 = FACE_OUTER_BOUND ( 'NONE', #14673, .T. ) ;
#14527 = EDGE_CURVE ( 'NONE', #8525, #4972, #20320, .T. ) ;
#14528 = EDGE_CURVE ( 'NONE', #7376, #15831, #8276, .T. ) ;
#14529 = VERTEX_POINT ( 'NONE', #18709 ) ;
#14530 = CYLINDRICAL_SURFACE ( 'NONE', #11500, 36.76383501243555685 ) ;
#14531 = AXIS2_PLACEMENT_3D ( 'NONE', #6776, #20425, #13739 ) ;
#14532 = EDGE_CURVE ( 'NONE', #11692, #21115, #14969, .T. ) ;
#14533 = CIRCLE ( 'NONE', #5774, 34.00000000000000000 ) ;
#14534 = CARTESIAN_POINT ( 'NONE',  ( 7.392698783198288659, 40.00000000000000711, -52.71482400407168001 ) ) ;
#14535 = ORIENTED_EDGE ( 'NONE', *, *, #15319, .F. ) ;
#14536 = DIRECTION ( 'NONE',  ( 0.000000000000000000, -1.000000000000000000, 0.000000000000000000 ) ) ;
#14537 = CIRCLE ( 'NONE', #9814, 6.499999999999999112 ) ;
#14538 = DIRECTION ( 'NONE',  ( -1.000000000000000000, -1.208970125616044077E-17, 0.000000000000000000 ) ) ;
#14539 = CARTESIAN_POINT ( 'NONE',  ( 42.50000000000000711, -5.000000000000000000, 41.00000000000000711 ) ) ;
#14540 = VECTOR ( 'NONE', #22329, 1000.000000000000000 ) ;
#14541 = ORIENTED_EDGE ( 'NONE', *, *, #2927, .T. ) ;
#14542 = CARTESIAN_POINT ( 'NONE',  ( 11.93830856187213207, 33.47097213929420434, 3.000000000000055955 ) ) ;
#14543 = CARTESIAN_POINT ( 'NONE',  ( -7.130208587515866725, 39.99999999999998579, 52.60396388218742203 ) ) ;
#14544 = VERTEX_POINT ( 'NONE', #2788 ) ;
#14545 = DIRECTION ( 'NONE',  ( 0.000000000000000000, 0.000000000000000000, -1.000000000000000000 ) ) ;
#14546 = CARTESIAN_POINT ( 'NONE',  ( -28.73837443790552371, 21.94460005644904754, -2.932164912090533981 ) ) ;
#14547 = CARTESIAN_POINT ( 'NONE',  ( 9.000000000000005329, 12.49999999999999467, -3.000000000000000000 ) ) ;
#14548 = DIRECTION ( 'NONE',  ( 0.000000000000000000, 0.000000000000000000, 1.000000000000000000 ) ) ;
#14549 = ORIENTED_EDGE ( 'NONE', *, *, #163, .T. ) ;
#14550 = LINE ( 'NONE', #14770, #20015 ) ;
#14551 = CARTESIAN_POINT ( 'NONE',  ( 36.06598984771573413, 10.00000000000000000, 48.42385786802029912 ) ) ;
#14552 = CARTESIAN_POINT ( 'NONE',  ( -0.5415566488456911021, 39.99826507375607321, -49.15084919631396332 ) ) ;
#14553 = ORIENTED_EDGE ( 'NONE', *, *, #3289, .T. ) ;
#14554 = EDGE_CURVE ( 'NONE', #3760, #10900, #8961, .T. ) ;
#14555 = VECTOR ( 'NONE', #19169, 1000.000000000000000 ) ;
#14556 = CARTESIAN_POINT ( 'NONE',  ( 5.999999999999998224, 20.00000000000000000, -5.999999999999999112 ) ) ;
#14557 = CARTESIAN_POINT ( 'NONE',  ( -22.98755168577401520, -22.97438720605754625, -2.999999999999971578 ) ) ;
#14558 = AXIS2_PLACEMENT_3D ( 'NONE', #3149, #12079, #10119 ) ;
#14559 = VECTOR ( 'NONE', #20465, 1000.000000000000000 ) ;
#14560 = AXIS2_PLACEMENT_3D ( 'NONE', #5985, #21924, #2559 ) ;
#14561 = ORIENTED_EDGE ( 'NONE', *, *, #3684, .T. ) ;
#14562 = VERTEX_POINT ( 'NONE', #11932 ) ;
#14563 = ORIENTED_EDGE ( 'NONE', *, *, #13539, .F. ) ;
#14564 =( NAMED_UNIT ( * ) SI_UNIT ( $, .STERADIAN. ) SOLID_ANGLE_UNIT ( ) );
#14565 = EDGE_LOOP ( 'NONE', ( #10786, #17993, #2215, #7710 ) ) ;
#14566 = CARTESIAN_POINT ( 'NONE',  ( 5.999999999999998224, 20.00000000000000000, -5.999999999999999112 ) ) ;
#14567 = DIRECTION ( 'NONE',  ( -1.000000000000000000, 0.000000000000000000, 0.000000000000000000 ) ) ;
#14568 = DIRECTION ( 'NONE',  ( -6.505213034913038160E-19, -3.903127820947822896E-18, -1.000000000000000000 ) ) ;
#14569 = AXIS2_PLACEMENT_3D ( 'NONE', #5014, #522, #7518 ) ;
#14570 = EDGE_LOOP ( 'NONE', ( #5576, #10270 ) ) ;
#14571 = DIRECTION ( 'NONE',  ( 0.000000000000000000, -1.000000000000000000, 0.000000000000000000 ) ) ;
#14573 = CIRCLE ( 'NONE', #10189, 2.999999999999999112 ) ;
#14572 = CARTESIAN_POINT ( 'NONE',  ( 90.00000000000000000, 39.97500000000000142, -2.500000000000003109 ) ) ;
#14574 = VERTEX_POINT ( 'NONE', #1284 ) ;
#14575 = CARTESIAN_POINT ( 'NONE',  ( 20.06142356895430368, -29.33203831401597483, 3.000000000000046629 ) ) ;
#14576 = EDGE_CURVE ( 'NONE', #10262, #22056, #22533, .T. ) ;
#14577 = CARTESIAN_POINT ( 'NONE',  ( -18.74703631669237680, 7.639653230112246618, -57.75728470191489095 ) ) ;
#14578 = AXIS2_PLACEMENT_3D ( 'NONE', #21379, #17937, #11053 ) ;
#14579 = PRODUCT_RELATED_PRODUCT_CATEGORY ( 'part', '', ( #891 ) ) ;
#14580 = DIRECTION ( 'NONE',  ( 0.000000000000000000, 0.000000000000000000, 1.000000000000000000 ) ) ;
#14581 = EDGE_LOOP ( 'NONE', ( #15835, #13135, #2794, #14050 ) ) ;
#14582 = LINE ( 'NONE', #5650, #9832 ) ;
#14583 = ORIENTED_EDGE ( 'NONE', *, *, #9336, .T. ) ;
#14584 = DIRECTION ( 'NONE',  ( 1.067522139062650671E-15, 0.000000000000000000, -1.000000000000000000 ) ) ;
#14585 = DIRECTION ( 'NONE',  ( -1.000000000000000000, 0.000000000000000000, 0.000000000000000000 ) ) ;
#14586 = DIRECTION ( 'NONE',  ( 0.000000000000000000, 0.000000000000000000, -1.000000000000000000 ) ) ;
#14587 = EDGE_CURVE ( 'NONE', #3870, #12877, #2766, .T. ) ;
#14588 = ORIENTED_EDGE ( 'NONE', *, *, #18029, .T. ) ;
#14589 = DIRECTION ( 'NONE',  ( 0.000000000000000000, -1.000000000000000000, 0.000000000000000000 ) ) ;
#14590 = CARTESIAN_POINT ( 'NONE',  ( 90.00000000000000000, 28.00000000000000000, -2.500000000000003109 ) ) ;
#14591 = DIRECTION ( 'NONE',  ( -6.505213034913038160E-19, -3.903127820947822896E-18, -1.000000000000000000 ) ) ;
#14592 = CARTESIAN_POINT ( 'NONE',  ( 4.683984772515711316E-15, 6.000000000000019540, -17.00000000000000355 ) ) ;
#14593 = AXIS2_PLACEMENT_3D ( 'NONE', #2248, #16213, #11059 ) ;
#14594 = VECTOR ( 'NONE', #20428, 999.9999999999998863 ) ;
#14595 = ORIENTED_EDGE ( 'NONE', *, *, #15041, .F. ) ;
#14596 = ORIENTED_EDGE ( 'NONE', *, *, #189, .T. ) ;
#14597 = EDGE_CURVE ( 'NONE', #8088, #19656, #16873, .T. ) ;
#14598 = EDGE_LOOP ( 'NONE', ( #16788, #10251, #12608, #18745 ) ) ;
#14599 = ORIENTED_EDGE ( 'NONE', *, *, #6654, .F. ) ;
#14600 = DIRECTION ( 'NONE',  ( -1.000000000000000000, 0.000000000000000000, 0.000000000000000000 ) ) ;
#14601 = CARTESIAN_POINT ( 'NONE',  ( -11.52370268861635161, 39.05614286682681779, -55.22012726398858717 ) ) ;
#14602 = CARTESIAN_POINT ( 'NONE',  ( -18.22261011550273224, -31.92986134326242365, -2.800654218530485018 ) ) ;
#14603 = VERTEX_POINT ( 'NONE', #6565 ) ;
#14604 = CARTESIAN_POINT ( 'NONE',  ( -11.51194040401124319, 39.05862814753013623, -55.21283662269279091 ) ) ;
#14605 = DIRECTION ( 'NONE',  ( 0.000000000000000000, 1.000000000000000000, 0.000000000000000000 ) ) ;
#14606 = EDGE_CURVE ( 'NONE', #21700, #11088, #15543, .T. ) ;
#14607 = ORIENTED_EDGE ( 'NONE', *, *, #19179, .F. ) ;
#14608 = DIRECTION ( 'NONE',  ( 0.000000000000000000, -1.000000000000000000, 0.000000000000000000 ) ) ;
#14609 = DIRECTION ( 'NONE',  ( 0.000000000000000000, 0.000000000000000000, -1.000000000000000000 ) ) ;
#14610 = CARTESIAN_POINT ( 'NONE',  ( -30.00000000000001421, 20.00000000000000711, -105.0000000000000142 ) ) ;
#14611 = CARTESIAN_POINT ( 'NONE',  ( 5.093313992686365310, 32.09841355225995585, -2.999999999999971578 ) ) ;
#14612 = LINE ( 'NONE', #12997, #8783 ) ;
#14613 = CARTESIAN_POINT ( 'NONE',  ( -2.881565232080841810, 39.80724445179826887, 51.34429047750199970 ) ) ;
#14614 = CARTESIAN_POINT ( 'NONE',  ( -13.33780792070363219, 2.142135623730927918, -45.06383732350883520 ) ) ;
#14615 = ORIENTED_EDGE ( 'NONE', *, *, #20849, .T. ) ;
#14616 = EDGE_LOOP ( 'NONE', ( #20223, #17053, #8777, #19089 ) ) ;
#14617 = EDGE_CURVE ( 'NONE', #3398, #17095, #16760, .T. ) ;
#14618 = CIRCLE ( 'NONE', #22336, 43.25806096964026892 ) ;
#14619 = ORIENTED_EDGE ( 'NONE', *, *, #19823, .F. ) ;
#14620 = DIRECTION ( 'NONE',  ( 6.505213034913038160E-19, 3.903127820947822896E-18, 1.000000000000000000 ) ) ;
#14621 = LINE ( 'NONE', #21743, #20047 ) ;
#14622 = ADVANCED_FACE ( 'NONE', ( #1071 ), #3121, .T. ) ;
#14623 = EDGE_CURVE ( 'NONE', #18681, #15589, #22381, .T. ) ;
#14624 = CIRCLE ( 'NONE', #4777, 19.11328065563151668 ) ;
#14625 = CARTESIAN_POINT ( 'NONE',  ( -2.999999999999999112, 16.00000000000000000, 6.485281374238567764 ) ) ;
#14626 = DIRECTION ( 'NONE',  ( 1.000000000000000000, -0.000000000000000000, -1.445602896647339163E-16 ) ) ;
#14627 = CARTESIAN_POINT ( 'NONE',  ( -9.786528823783235964, 39.51685528920044277, -54.52238163179004005 ) ) ;
#14628 = CARTESIAN_POINT ( 'NONE',  ( -90.00000000000000000, 28.00000000000000000, 2.099999999999989875 ) ) ;
#14629 = DIRECTION ( 'NONE',  ( -0.000000000000000000, 1.000000000000000000, -0.000000000000000000 ) ) ;
#14630 = CARTESIAN_POINT ( 'NONE',  ( -1.387778780781445676E-14, 20.00000000000000000, 60.00200000000000244 ) ) ;
#14631 = VECTOR ( 'NONE', #7935, 1000.000000000000000 ) ;
#14632 = ORIENTED_EDGE ( 'NONE', *, *, #3810, .T. ) ;
#14633 = CARTESIAN_POINT ( 'NONE',  ( 10.50000000000024514, -2.516660498395250745, -100.0000000000000000 ) ) ;
#14634 = EDGE_CURVE ( 'NONE', #8988, #131, #6330, .T. ) ;
#14635 = CYLINDRICAL_SURFACE ( 'NONE', #21963, 19.11328065563152023 ) ;
#14636 = FACE_OUTER_BOUND ( 'NONE', #9641, .T. ) ;
#14637 = CARTESIAN_POINT ( 'NONE',  ( 35.00000000000001421, 0.000000000000000000, 4.999999999999997335 ) ) ;
#14638 = VERTEX_POINT ( 'NONE', #13628 ) ;
#14639 = DIRECTION ( 'NONE',  ( -1.209647751973867239E-17, -1.000000000000000000, 3.903127820947822896E-18 ) ) ;
#14640 = ORIENTED_EDGE ( 'NONE', *, *, #13793, .F. ) ;
#14641 = LINE ( 'NONE', #19925, #5302 ) ;
#14642 = DIRECTION ( 'NONE',  ( -6.505213034913038160E-19, -3.903127820947822896E-18, -1.000000000000000000 ) ) ;
#14643 = AXIS2_PLACEMENT_3D ( 'NONE', #4809, #11677, #10282 ) ;
#14644 = EDGE_LOOP ( 'NONE', ( #8944, #10268, #3493, #20350 ) ) ;
#14645 = FACE_OUTER_BOUND ( 'NONE', #698, .T. ) ;
#14646 = CARTESIAN_POINT ( 'NONE',  ( 4.925985921465350081, 39.99999999999998579, -51.57279956358078010 ) ) ;
#14647 = ORIENTED_EDGE ( 'NONE', *, *, #9026, .F. ) ;
#14648 = CARTESIAN_POINT ( 'NONE',  ( 0.4054037750498698522, 39.99903173806880829, -49.04694161421060983 ) ) ;
#14649 = CARTESIAN_POINT ( 'NONE',  ( 10.06223851446352668, 39.28158160658968967, 54.67678195792215945 ) ) ;
#14650 = DIRECTION ( 'NONE',  ( 1.000000000000000000, 0.000000000000000000, 0.000000000000000000 ) ) ;
#14651 = ORIENTED_EDGE ( 'NONE', *, *, #7245, .T. ) ;
#14652 = CARTESIAN_POINT ( 'NONE',  ( 1.110223024625156540E-13, -5.551115123125782702E-14, -6.999999999999950262 ) ) ;
#14653 = AXIS2_PLACEMENT_3D ( 'NONE', #22061, #16790, #6355 ) ;
#14654 = CARTESIAN_POINT ( 'NONE',  ( -7.505578006075232622, 1.461761173328252283, -55.63523492904088386 ) ) ;
#14655 = ORIENTED_EDGE ( 'NONE', *, *, #3992, .F. ) ;
#14656 = CARTESIAN_POINT ( 'NONE',  ( -20.17230487860800636, -25.34312177887357365, -6.999999999999950262 ) ) ;
#14657 = EDGE_CURVE ( 'NONE', #15589, #16403, #7131, .T. ) ;
#14658 = CYLINDRICAL_SURFACE ( 'NONE', #4231, 12.00000000000000000 ) ;
#14659 = CIRCLE ( 'NONE', #392, 2.099999999999990763 ) ;
#14660 = EDGE_CURVE ( 'NONE', #5292, #3151, #1744, .T. ) ;
#14661 = DIRECTION ( 'NONE',  ( 0.000000000000000000, -1.000000000000000000, 0.000000000000000000 ) ) ;
#14662 = ORIENTED_EDGE ( 'NONE', *, *, #13419, .T. ) ;
#14663 = DIRECTION ( 'NONE',  ( -0.000000000000000000, -1.000000000000000000, -0.000000000000000000 ) ) ;
#14664 = DIRECTION ( 'NONE',  ( -0.000000000000000000, -0.000000000000000000, 1.000000000000000000 ) ) ;
#14665 = DIRECTION ( 'NONE',  ( -1.000000000000000000, -1.208970125616046080E-17, 6.505213034913038160E-19 ) ) ;
#14666 = DIRECTION ( 'NONE',  ( -0.9012767464701406661, 1.437462578140670496E-16, -0.4332438415860032643 ) ) ;
#14667 = ORIENTED_EDGE ( 'NONE', *, *, #20503, .T. ) ;
#14668 = FACE_OUTER_BOUND ( 'NONE', #17980, .T. ) ;
#14669 = ADVANCED_FACE ( 'NONE', ( #1854 ), #21102, .T. ) ;
#14670 = CARTESIAN_POINT ( 'NONE',  ( -14.68506606271061443, 23.08193591670981348, 45.68712064066591694 ) ) ;
#14671 = CARTESIAN_POINT ( 'NONE',  ( -35.00000000000058265, 26.00000000000000355, -55.00000000000076028 ) ) ;
#14672 = VERTEX_POINT ( 'NONE', #17649 ) ;
#14673 = EDGE_LOOP ( 'NONE', ( #11012, #22645, #22396, #5035, #370 ) ) ;
#14674 = VERTEX_POINT ( 'NONE', #4109 ) ;
#14675 = ORIENTED_EDGE ( 'NONE', *, *, #3810, .F. ) ;
#14676 = CARTESIAN_POINT ( 'NONE',  ( 12.24033418603698209, 35.84417766536505212, 58.14550894043698293 ) ) ;
#14677 = CARTESIAN_POINT ( 'NONE',  ( -13.00000000000011546, 42.51666049839536043, 60.00099999999999767 ) ) ;
#14678 = CARTESIAN_POINT ( 'NONE',  ( 6.383438919230843859E-14, -1.500000000000011768, -20.00000000000029488 ) ) ;
#14679 = DIRECTION ( 'NONE',  ( 6.505213034913038160E-19, 3.903127820947822896E-18, 1.000000000000000000 ) ) ;
#14680 = CARTESIAN_POINT ( 'NONE',  ( 35.00000000000001421, 4.000000000000028422, 10.00000000000000000 ) ) ;
#14681 = ORIENTED_EDGE ( 'NONE', *, *, #1377, .T. ) ;
#14682 = DIRECTION ( 'NONE',  ( 1.000000000000000000, 0.000000000000000000, 0.000000000000000000 ) ) ;
#14683 = DIRECTION ( 'NONE',  ( 6.505213034913038160E-19, 3.903127820947822896E-18, 1.000000000000000000 ) ) ;
#14684 = EDGE_LOOP ( 'NONE', ( #1086, #17977, #12960, #9540 ) ) ;
#14685 = DIRECTION ( 'NONE',  ( 1.000000000000000000, -0.000000000000000000, 0.000000000000000000 ) ) ;
#14686 = DIRECTION ( 'NONE',  ( -0.000000000000000000, -1.000000000000000000, -0.000000000000000000 ) ) ;
#14687 = AXIS2_PLACEMENT_3D ( 'NONE', #1501, #1730, #7000 ) ;
#14688 = CARTESIAN_POINT ( 'NONE',  ( 19.74829075628832697, 16.81150045999882892, -60.56179516789183737 ) ) ;
#14689 = EDGE_LOOP ( 'NONE', ( #20559, #614, #22461, #4853 ) ) ;
#14690 = DIRECTION ( 'NONE',  ( 0.000000000000000000, -1.000000000000000000, 0.000000000000000000 ) ) ;
#14691 = CARTESIAN_POINT ( 'NONE',  ( 3.469446951953614189E-15, 38.23275711891355400, 0.000000000000000000 ) ) ;
#14692 = ORIENTED_EDGE ( 'NONE', *, *, #10938, .F. ) ;
#14693 = CARTESIAN_POINT ( 'NONE',  ( 7.938322399560873599, 38.36220367130487574, 56.16250688145269976 ) ) ;
#14694 = CARTESIAN_POINT ( 'NONE',  ( -4.295527433237782828E-15, -1.236374842841486021, 48.24164917503448180 ) ) ;
#14695 = ORIENTED_EDGE ( 'NONE', *, *, #8040, .T. ) ;
#14696 = CARTESIAN_POINT ( 'NONE',  ( 11.93214024655333638, 36.05624711372924196, 58.01435237789500121 ) ) ;
#14697 = DIRECTION ( 'NONE',  ( 6.505213034913038160E-19, 3.903127820947822896E-18, 1.000000000000000000 ) ) ;
#14698 = CARTESIAN_POINT ( 'NONE',  ( 14.30127497006473547, 34.01755211514666399, -56.34491176086893205 ) ) ;
#14700 = VERTEX_POINT ( 'NONE', #12054 ) ;
#14699 = EDGE_CURVE ( 'NONE', #18704, #21119, #4953, .T. ) ;
#14701 = VECTOR ( 'NONE', #20695, 1000.000000000000000 ) ;
#14702 = ORIENTED_EDGE ( 'NONE', *, *, #1505, .F. ) ;
#14703 = ORIENTED_EDGE ( 'NONE', *, *, #9451, .F. ) ;
#14704 = EDGE_LOOP ( 'NONE', ( #17432, #13511, #22318, #10641 ) ) ;
#14705 = CARTESIAN_POINT ( 'NONE',  ( 10.08226496203362110, 39.27879523430843989, 54.68359763861834466 ) ) ;
#14706 = DIRECTION ( 'NONE',  ( 0.000000000000000000, 0.000000000000000000, -1.000000000000000000 ) ) ;
#14707 = EDGE_CURVE ( 'NONE', #14638, #22326, #21417, .T. ) ;
#14708 = CARTESIAN_POINT ( 'NONE',  ( -14.67611967928926475, 31.67162468655990182, -2.999999999999971578 ) ) ;
#14709 = EDGE_LOOP ( 'NONE', ( #14299, #16968, #12477, #14970 ) ) ;
#14710 = DIRECTION ( 'NONE',  ( -0.000000000000000000, 1.000000000000000000, -0.000000000000000000 ) ) ;
#14711 = ORIENTED_EDGE ( 'NONE', *, *, #22079, .T. ) ;
#14712 = DIRECTION ( 'NONE',  ( 0.000000000000000000, 0.000000000000000000, 1.000000000000000000 ) ) ;
#14713 = LINE ( 'NONE', #13326, #14559 ) ;
#14714 = DIRECTION ( 'NONE',  ( 0.000000000000000000, 0.000000000000000000, 1.000000000000000000 ) ) ;
#14715 = CARTESIAN_POINT ( 'NONE',  ( 25.00000000000000000, -20.00000000000000000, 6.487780019669002523E-15 ) ) ;
#14716 = CIRCLE ( 'NONE', #12520, 1.999999999999999778 ) ;
#14717 = CARTESIAN_POINT ( 'NONE',  ( -29.14949368109855143, 11.93972437435547640, -2.999999999999992450 ) ) ;
#14718 = CARTESIAN_POINT ( 'NONE',  ( -1.427812194317577887, 39.96253263129007394, 50.08434126564738165 ) ) ;
#14719 = CYLINDRICAL_SURFACE ( 'NONE', #2817, 49.99999999999998579 ) ;
#14720 = EDGE_CURVE ( 'NONE', #10179, #1794, #11538, .T. ) ;
#14721 = ORIENTED_EDGE ( 'NONE', *, *, #7964, .T. ) ;
#14722 = ORIENTED_EDGE ( 'NONE', *, *, #10249, .F. ) ;
#14723 = VERTEX_POINT ( 'NONE', #19276 ) ;
#14724 = EDGE_CURVE ( 'NONE', #18953, #7816, #8834, .T. ) ;
#14725 = CYLINDRICAL_SURFACE ( 'NONE', #17717, 17.00000000000000000 ) ;
#14726 = AXIS2_PLACEMENT_3D ( 'NONE', #14132, #15751, #15636 ) ;
#14727 = DIRECTION ( 'NONE',  ( -1.000000000000000000, 2.128324605523459973E-14, 0.000000000000000000 ) ) ;
#14728 = CARTESIAN_POINT ( 'NONE',  ( 2.589862425843529881, 0.1394011931330937371, -50.61994180264545662 ) ) ;
#14729 = AXIS2_PLACEMENT_3D ( 'NONE', #1862, #5196, #18945 ) ;
#14730 = CARTESIAN_POINT ( 'NONE',  ( 19.59430950039317665, -28.88846368933348074, -2.999999999999999112 ) ) ;
#14731 = DIRECTION ( 'NONE',  ( -0.000000000000000000, -0.000000000000000000, 1.000000000000000000 ) ) ;
#14732 = DIRECTION ( 'NONE',  ( 0.000000000000000000, 0.000000000000000000, 1.000000000000000000 ) ) ;
#14733 = CARTESIAN_POINT ( 'NONE',  ( -4.750159105397525394, 39.43751337119567779, -52.76321094647789778 ) ) ;
#14734 = DIRECTION ( 'NONE',  ( -1.000000000000000000, 0.000000000000000000, 0.000000000000000000 ) ) ;
#14735 = DIRECTION ( 'NONE',  ( -6.505213034913038160E-19, -3.903127820947822896E-18, -1.000000000000000000 ) ) ;
#14736 = EDGE_CURVE ( 'NONE', #768, #13884, #17749, .T. ) ;
#14737 = VERTEX_POINT ( 'NONE', #5077 ) ;
#14738 = CARTESIAN_POINT ( 'NONE',  ( -19.99999999999969091, -2.554026978681552118E-14, -2.999999999999971578 ) ) ;
#14739 = DIRECTION ( 'NONE',  ( 0.000000000000000000, -1.000000000000000000, 0.000000000000000000 ) ) ;
#14740 = DIRECTION ( 'NONE',  ( -0.000000000000000000, 1.000000000000000000, -0.000000000000000000 ) ) ;
#14741 = ORIENTED_EDGE ( 'NONE', *, *, #17581, .T. ) ;
#14742 = CIRCLE ( 'NONE', #129, 1.000000000000000888 ) ;
#14743 = VERTEX_POINT ( 'NONE', #235 ) ;
#14744 = B_SPLINE_CURVE_WITH_KNOTS ( 'NONE', 3,
 ( #12673, #14068, #19692, #10965 ),
 .UNSPECIFIED., .F., .F.,
 ( 4, 4 ),
 ( 0.001875451646902760077, 0.003761979286331185689 ),
 .UNSPECIFIED. ) ;
#14745 = DIRECTION ( 'NONE',  ( 6.505213034913038160E-19, 3.903127820947822896E-18, 1.000000000000000000 ) ) ;
#14746 = DIRECTION ( 'NONE',  ( 0.000000000000000000, 0.000000000000000000, 1.000000000000000000 ) ) ;
#14747 = CIRCLE ( 'NONE', #18425, 1.000000000000000888 ) ;
#14748 = ADVANCED_FACE ( 'NONE', ( #21524 ), #19949, .T. ) ;
#14749 = EDGE_CURVE ( 'NONE', #6570, #9329, #19234, .T. ) ;
#14750 = AXIS2_PLACEMENT_3D ( 'NONE', #11794, #19030, #3099 ) ;
#14751 = VERTEX_POINT ( 'NONE', #19048 ) ;
#14752 = CARTESIAN_POINT ( 'NONE',  ( -17.79500259159599906, -31.47514467962714235, 2.932460736555821956 ) ) ;
#14753 = AXIS2_PLACEMENT_3D ( 'NONE', #2145, #21168, #1697 ) ;
#14754 = EDGE_CURVE ( 'NONE', #5656, #12273, #9378, .T. ) ;
#14755 = CARTESIAN_POINT ( 'NONE',  ( 4.416369897321547278, 40.00000000000000000, -51.31508173270569984 ) ) ;
#14756 = VERTEX_POINT ( 'NONE', #10314 ) ;
#14757 = CARTESIAN_POINT ( 'NONE',  ( 8.492273976632109367, 39.51732055898253293, -54.09038579245198264 ) ) ;
#14758 = DIRECTION ( 'NONE',  ( -6.505213034913038160E-19, -3.903127820947822896E-18, -1.000000000000000000 ) ) ;
#14759 = VECTOR ( 'NONE', #7672, 1000.000000000000000 ) ;
#14760 = DIRECTION ( 'NONE',  ( 1.000000000000000000, 1.208970125616063490E-17, 0.000000000000000000 ) ) ;
#14761 = AXIS2_PLACEMENT_3D ( 'NONE', #1011, #9837, #11434 ) ;
#14762 = EDGE_CURVE ( 'NONE', #10413, #9999, #8942, .T. ) ;
#14763 = CARTESIAN_POINT ( 'NONE',  ( 1.387778780781445676E-14, 40.00000000000000000, 48.73397172404482802 ) ) ;
#14764 = DIRECTION ( 'NONE',  ( 1.000000000000000000, 1.208970125616053475E-17, 0.000000000000000000 ) ) ;
#14765 = CONICAL_SURFACE ( 'NONE', #1601, 15.00000000000000000, 0.7853981633974552734 ) ;
#14766 = CARTESIAN_POINT ( 'NONE',  ( -3.997613013123614056, 39.99999999999999289, 51.09533622492809712 ) ) ;
#14767 = DIRECTION ( 'NONE',  ( -0.000000000000000000, -0.000000000000000000, -1.000000000000000000 ) ) ;
#14768 = EDGE_CURVE ( 'NONE', #19011, #5386, #17425, .T. ) ;
#14769 = ORIENTED_EDGE ( 'NONE', *, *, #21359, .F. ) ;
#14770 = CARTESIAN_POINT ( 'NONE',  ( -35.00000000000000000, 39.00000000000000711, 50.00000000000000000 ) ) ;
#14771 = DIRECTION ( 'NONE',  ( -6.505213034913038160E-19, -3.903127820947822896E-18, -1.000000000000000000 ) ) ;
#14772 = CARTESIAN_POINT ( 'NONE',  ( -34.99999999999999289, 5.000000000000000000, -9.000000000000065725 ) ) ;
#14773 = ORIENTED_EDGE ( 'NONE', *, *, #3170, .F. ) ;
#14774 = CARTESIAN_POINT ( 'NONE',  ( 1.734723475976807094E-14, -20.00000000000000000, 20.71067811865476216 ) ) ;
#14775 = CIRCLE ( 'NONE', #21745, 30.00000000000000000 ) ;
#14776 = DIRECTION ( 'NONE',  ( 1.445602896647339410E-16, 0.000000000000000000, 1.000000000000000000 ) ) ;
#14777 = DIRECTION ( 'NONE',  ( -1.000000000000000000, -1.208970125616081209E-17, 0.000000000000000000 ) ) ;
#14778 = EDGE_CURVE ( 'NONE', #15385, #15800, #15919, .T. ) ;
#14779 = CIRCLE ( 'NONE', #20627, 51.00000000000002132 ) ;
#14780 = CONICAL_SURFACE ( 'NONE', #6739, 10.00000000000000000, 0.7853981633974447263 ) ;
#14782 = ADVANCED_FACE ( 'NONE', ( #7010 ), #12793, .F. ) ;
#14781 = EDGE_LOOP ( 'NONE', ( #14675, #19232, #18229, #10773 ) ) ;
#14783 = VERTEX_POINT ( 'NONE', #12161 ) ;
#14784 = ORIENTED_EDGE ( 'NONE', *, *, #3821, .T. ) ;
#14785 = CARTESIAN_POINT ( 'NONE',  ( 19.43416121892454385, 24.82270088923176132, 60.48577746614103035 ) ) ;
#14786 = CARTESIAN_POINT ( 'NONE',  ( 6.661198439252276948, -4.819795714535265674, 49.67388352367134985 ) ) ;
#14787 = CARTESIAN_POINT ( 'NONE',  ( -10.50000000000012079, 42.51666049839536043, 100.0000000000000000 ) ) ;
#14788 = DIRECTION ( 'NONE',  ( 0.000000000000000000, 0.000000000000000000, 1.000000000000000000 ) ) ;
#14789 = AXIS2_PLACEMENT_3D ( 'NONE', #17037, #15194, #10043 ) ;
#14790 = DIRECTION ( 'NONE',  ( -0.000000000000000000, 1.000000000000000000, -0.000000000000000000 ) ) ;
#14791 = EDGE_LOOP ( 'NONE', ( #18293, #3746, #5322, #20913 ) ) ;
#14792 = LINE ( 'NONE', #20088, #18638 ) ;
#14793 = DIRECTION ( 'NONE',  ( -6.505213034913038160E-19, -3.903127820947822896E-18, -1.000000000000000000 ) ) ;
#14794 = VERTEX_POINT ( 'NONE', #15704 ) ;
#14795 = CARTESIAN_POINT ( 'NONE',  ( -14.87996495114181172, 18.06670563205964797, -45.77322900830824892 ) ) ;
#14796 = CYLINDRICAL_SURFACE ( 'NONE', #8638, 2.500000000000002220 ) ;
#14797 = CARTESIAN_POINT ( 'NONE',  ( 2.999999999999998224, 22.00000000000000000, 6.485281374238567764 ) ) ;
#14798 = VERTEX_POINT ( 'NONE', #3468 ) ;
#14799 = CARTESIAN_POINT ( 'NONE',  ( -1.387778780781445518E-14, 20.00000000000000355, 105.0000000000000142 ) ) ;
#14800 = CARTESIAN_POINT ( 'NONE',  ( 35.00000000000000000, -4.999999999999997335, 4.258610482196280173E-15 ) ) ;
#14801 = ORIENTED_EDGE ( 'NONE', *, *, #6047, .T. ) ;
#14802 = CARTESIAN_POINT ( 'NONE',  ( 5.204758277554829782, 39.83793674575848343, 52.32476555783389927 ) ) ;
#14803 = ORIENTED_EDGE ( 'NONE', *, *, #680, .F. ) ;
#14804 = DIRECTION ( 'NONE',  ( -0.000000000000000000, 1.000000000000000000, -0.000000000000000000 ) ) ;
#14805 = CARTESIAN_POINT ( 'NONE',  ( -30.48934413892756368, 16.99647590252650886, -2.999999999999995559 ) ) ;
#14806 = CIRCLE ( 'NONE', #16655, 3.999999999999996447 ) ;
#14807 = CARTESIAN_POINT ( 'NONE',  ( 27.62019382530525391, -4.341204441673157888, -2.999999999999999112 ) ) ;
#14808 = AXIS2_PLACEMENT_3D ( 'NONE', #20945, #3755, #2023 ) ;
#14810 = EDGE_CURVE ( 'NONE', #3413, #9068, #15902, .T. ) ;
#14809 = ORIENTED_EDGE ( 'NONE', *, *, #13920, .T. ) ;
#14811 = CIRCLE ( 'NONE', #14444, 10.00000000000000000 ) ;
#14812 = ORIENTED_EDGE ( 'NONE', *, *, #15162, .F. ) ;
#14813 = VERTEX_POINT ( 'NONE', #4451 ) ;
#14814 = VERTEX_POINT ( 'NONE', #14628 ) ;
#14815 = CARTESIAN_POINT ( 'NONE',  ( 2.220446049250313081E-13, -8.326672684688674053E-14, 2.800654218530498785 ) ) ;
#14816 = ADVANCED_FACE ( 'NONE', ( #20034 ), #13134, .T. ) ;
#14817 = ORIENTED_EDGE ( 'NONE', *, *, #5270, .T. ) ;
#14818 = CARTESIAN_POINT ( 'NONE',  ( 2.220446049250313081E-13, -25.00000000000007816, -4.999999999999962697 ) ) ;
#14819 = CARTESIAN_POINT ( 'NONE',  ( 0.000000000000000000, 15.00000000000000355, 0.000000000000000000 ) ) ;
#14820 = ORIENTED_EDGE ( 'NONE', *, *, #15001, .T. ) ;
#14821 = AXIS2_PLACEMENT_3D ( 'NONE', #9183, #17774, #2082 ) ;
#14822 = CIRCLE ( 'NONE', #187, 2.499999999999998668 ) ;
#14823 = ORIENTED_EDGE ( 'NONE', *, *, #7740, .T. ) ;
#14824 = CARTESIAN_POINT ( 'NONE',  ( -42.50000000000000711, -9.600000000000001421, 47.50000000000000711 ) ) ;
#14825 = DIRECTION ( 'NONE',  ( 8.659560562354903276E-17, -0.7071067811865500152, 0.7071067811865451302 ) ) ;
#14826 = DIRECTION ( 'NONE',  ( -6.505213034913038160E-19, -3.903127820947822896E-18, -1.000000000000000000 ) ) ;
#14827 = CARTESIAN_POINT ( 'NONE',  ( 11.85401191286916678, 32.83234229683709771, -2.999999999999995559 ) ) ;
#14828 = EDGE_CURVE ( 'NONE', #15027, #11046, #18512, .T. ) ;
#14829 = CIRCLE ( 'NONE', #9725, 2.999999999999999112 ) ;
#14830 = ADVANCED_FACE ( 'NONE', ( #22095 ), #15201, .F. ) ;
#14831 = CARTESIAN_POINT ( 'NONE',  ( -4.750178577765296950, 39.43750913335933461, 52.76318739013298398 ) ) ;
#14832 = FACE_OUTER_BOUND ( 'NONE', #17355, .T. ) ;
#14833 = CIRCLE ( 'NONE', #4985, 22.00000000000000000 ) ;
#14834 = VERTEX_POINT ( 'NONE', #11429 ) ;
#14835 = ORIENTED_EDGE ( 'NONE', *, *, #10505, .F. ) ;
#14836 = ORIENTED_EDGE ( 'NONE', *, *, #18832, .F. ) ;
#14837 = CARTESIAN_POINT ( 'NONE',  ( -17.96966555604169713, 28.82469637350494907, 60.10139901455269040 ) ) ;
#14838 = VECTOR ( 'NONE', #6180, 1000.000000000000000 ) ;
#14839 = DIRECTION ( 'NONE',  ( -6.505213034913038160E-19, -3.903127820947822896E-18, -1.000000000000000000 ) ) ;
#14840 = PLANE ( 'NONE',  #21142 ) ;
#14841 = CARTESIAN_POINT ( 'NONE',  ( 8.331955809010601399, 38.18181818181818699, 56.36098470834073026 ) ) ;
#14842 = CARTESIAN_POINT ( 'NONE',  ( -9.857944917841409804, 0.2919354798322641997, -54.29891737064848201 ) ) ;
#14843 = AXIS2_PLACEMENT_3D ( 'NONE', #4623, #13288, #20764 ) ;
#14844 = CIRCLE ( 'NONE', #8654, 2.500000000000002220 ) ;
#14845 = DIRECTION ( 'NONE',  ( -1.000000000000000000, -1.208970125616081209E-17, 0.000000000000000000 ) ) ;
#14846 = CIRCLE ( 'NONE', #2809, 19.11328065563152379 ) ;
#14847 = DIRECTION ( 'NONE',  ( 6.505213034913038160E-19, 3.903127820947822896E-18, 1.000000000000000000 ) ) ;
#14848 = EDGE_CURVE ( 'NONE', #9194, #10462, #12287, .T. ) ;
#14849 = CIRCLE ( 'NONE', #5002, 3.399999999999995026 ) ;
#14850 = ORIENTED_EDGE ( 'NONE', *, *, #11406, .T. ) ;
#14851 = CARTESIAN_POINT ( 'NONE',  ( -35.99819890246949683, 7.463862311151203244, -2.800654218530485018 ) ) ;
#14852 = CARTESIAN_POINT ( 'NONE',  ( 13.56209497734233871, 5.196600802614999459, 56.07847567638239639 ) ) ;
#14853 = CARTESIAN_POINT ( 'NONE',  ( 30.60042966911727547, 7.474202570536048640, -6.999999999999950262 ) ) ;
#14854 = EDGE_CURVE ( 'NONE', #13173, #12588, #2961, .T. ) ;
#14855 = CIRCLE ( 'NONE', #1715, 19.11328065563151313 ) ;
#14856 = EDGE_LOOP ( 'NONE', ( #5754, #14246, #21195, #10756, #16253, #4162 ) ) ;
#14857 = FACE_OUTER_BOUND ( 'NONE', #7570, .T. ) ;
#14858 = DIRECTION ( 'NONE',  ( 6.505213034913038160E-19, 3.903127820947822896E-18, 1.000000000000000000 ) ) ;
#14859 = CARTESIAN_POINT ( 'NONE',  ( 2.602085213965210642E-15, -0.9047447100419790944, 0.000000000000000000 ) ) ;
#14860 = ORIENTED_EDGE ( 'NONE', *, *, #12408, .T. ) ;
#14861 = AXIS2_PLACEMENT_3D ( 'NONE', #327, #7318, #14283 ) ;
#14862 = DIRECTION ( 'NONE',  ( -1.000000000000000000, -1.208970125616044077E-17, 0.000000000000000000 ) ) ;
#14863 = EDGE_CURVE ( 'NONE', #4837, #15126, #17766, .T. ) ;
#14864 = CARTESIAN_POINT ( 'NONE',  ( -1.387778780781445676E-14, 40.00000000000000000, -48.73397172404481381 ) ) ;
#14865 = ORIENTED_EDGE ( 'NONE', *, *, #12096, .F. ) ;
#14866 = CARTESIAN_POINT ( 'NONE',  ( 2.217097043154531821, 39.97039924782914966, -50.37983924381441625 ) ) ;
#14867 = CIRCLE ( 'NONE', #22594, 36.76383501243555685 ) ;
#14868 = DIRECTION ( 'NONE',  ( 0.000000000000000000, 0.000000000000000000, 1.000000000000000000 ) ) ;
#14869 = CARTESIAN_POINT ( 'NONE',  ( 35.00000000000000711, 40.00000000000000000, 58.99999999999995026 ) ) ;
#14870 = DIRECTION ( 'NONE',  ( -6.505213034913038160E-19, -3.903127820947822896E-18, -1.000000000000000000 ) ) ;
#14871 = EDGE_CURVE ( 'NONE', #18756, #1286, #13724, .T. ) ;
#14872 = CARTESIAN_POINT ( 'NONE',  ( 11.53082054500845999, 39.05546563731292764, -55.22070542780790703 ) ) ;
#14873 = CARTESIAN_POINT ( 'NONE',  ( -9.689843208404422370, 39.33333333333333570, 54.54983754392743833 ) ) ;
#14874 = DIRECTION ( 'NONE',  ( -0.000000000000000000, -1.000000000000000000, -0.000000000000000000 ) ) ;
#14875 = ORIENTED_EDGE ( 'NONE', *, *, #19638, .F. ) ;
#14876 = DIRECTION ( 'NONE',  ( 6.505213034913038160E-19, 3.903127820947822896E-18, 1.000000000000000000 ) ) ;
#14877 = AXIS2_PLACEMENT_3D ( 'NONE', #12478, #19388, #2295 ) ;
#14878 = CARTESIAN_POINT ( 'NONE',  ( -13.85640646055073333, -25.00000000000000000, -8.000000000000493827 ) ) ;
#14879 = DIRECTION ( 'NONE',  ( 6.505213034913038160E-19, 3.903127820947822896E-18, 1.000000000000000000 ) ) ;
#14880 = ORIENTED_EDGE ( 'NONE', *, *, #7208, .T. ) ;
#14881 = LINE ( 'NONE', #9415, #10892 ) ;
#14882 = CARTESIAN_POINT ( 'NONE',  ( -14.50678847729823850, 23.83439465050324912, 45.60743157421821792 ) ) ;
#14883 = DIRECTION ( 'NONE',  ( -6.505213034913038160E-19, -3.903127820947822896E-18, -1.000000000000000000 ) ) ;
#14884 = VECTOR ( 'NONE', #20550, 1000.000000000000114 ) ;
#14885 = AXIS2_PLACEMENT_3D ( 'NONE', #14677, #4158, #9085 ) ;
#14886 = ORIENTED_EDGE ( 'NONE', *, *, #5687, .F. ) ;
#14887 = AXIS2_PLACEMENT_3D ( 'NONE', #6560, #13521, #4839 ) ;
#14888 = EDGE_CURVE ( 'NONE', #19609, #3399, #12636, .T. ) ;
#14889 = VECTOR ( 'NONE', #2982, 1000.000000000000000 ) ;
#14890 = VERTEX_POINT ( 'NONE', #5931 ) ;
#14891 = DIRECTION ( 'NONE',  ( -0.9956380956557518980, 0.09323724882972866945, -0.003405570385571841507 ) ) ;
#14892 = ORIENTED_EDGE ( 'NONE', *, *, #16106, .T. ) ;
#14893 = CARTESIAN_POINT ( 'NONE',  ( 18.50805780747142393, 27.59542556733954655, 60.24679276096815528 ) ) ;
#14894 = CYLINDRICAL_SURFACE ( 'NONE', #17240, 0.9999999999999974465 ) ;
#14895 = DIRECTION ( 'NONE',  ( 1.000000000000000000, 0.000000000000000000, 0.000000000000000000 ) ) ;
#14896 = FACE_OUTER_BOUND ( 'NONE', #16766, .T. ) ;
#14897 = CARTESIAN_POINT ( 'NONE',  ( -1.079570778443290191, 5.000568130954873070, -38.73482392062542345 ) ) ;
#14898 = ORIENTED_EDGE ( 'NONE', *, *, #2201, .T. ) ;
#14899 = DIRECTION ( 'NONE',  ( 0.000000000000000000, 0.000000000000000000, -1.000000000000000000 ) ) ;
#14900 = CARTESIAN_POINT ( 'NONE',  ( 35.16985127952418111, 10.70799354677351367, -2.800654218530464146 ) ) ;
#14901 = EDGE_LOOP ( 'NONE', ( #12769, #16053, #162, #18986 ) ) ;
#14902 = EDGE_CURVE ( 'NONE', #11055, #2840, #20261, .T. ) ;
#14903 = ADVANCED_FACE ( 'NONE', ( #20376 ), #9830, .F. ) ;
#14904 = DIRECTION ( 'NONE',  ( -1.000000000000000000, -1.208970125616060101E-17, 6.505213034913038160E-19 ) ) ;
#14905 = ADVANCED_FACE ( 'NONE', ( #6169 ), #4681, .F. ) ;
#14906 = DIRECTION ( 'NONE',  ( -0.000000000000000000, -1.000000000000000000, -0.000000000000000000 ) ) ;
#14907 = EDGE_LOOP ( 'NONE', ( #13808, #20948, #13686, #1354 ) ) ;
#14908 = CARTESIAN_POINT ( 'NONE',  ( 32.20238537491815123, 4.080045426412798548, 2.999999999999995559 ) ) ;
#14909 = CARTESIAN_POINT ( 'NONE',  ( 3.210361346424027484, 39.75306810546534564, -52.30715206667685635 ) ) ;
#14910 = VECTOR ( 'NONE', #8795, 1000.000000000000000 ) ;
#14911 = ORIENTED_EDGE ( 'NONE', *, *, #8775, .T. ) ;
#14912 = CARTESIAN_POINT ( 'NONE',  ( 2.585597902343947566E-15, -8.251288694035734395, 0.000000000000000000 ) ) ;
#14913 = CARTESIAN_POINT ( 'NONE',  ( -1.438799862756543035, -1.268859023760806837, -49.24077205406572944 ) ) ;
#14914 = AXIS2_PLACEMENT_3D ( 'NONE', #16666, #4534, #16999 ) ;
#14915 = VERTEX_POINT ( 'NONE', #16474 ) ;
#14916 = AXIS2_PLACEMENT_3D ( 'NONE', #9517, #16497, #803 ) ;
#14917 = UNCERTAINTY_MEASURE_WITH_UNIT (LENGTH_MEASURE( 1.000000000000000082E-05 ), #4491, 'distance_accuracy_value', 'NONE');
#14918 = CIRCLE ( 'NONE', #10528, 1.000000000000000888 ) ;
#14919 = DIRECTION ( 'NONE',  ( 0.000000000000000000, 0.000000000000000000, 1.000000000000000000 ) ) ;
#14920 = EDGE_CURVE ( 'NONE', #6602, #21037, #5698, .T. ) ;
#14921 = CARTESIAN_POINT ( 'NONE',  ( -7.094908322883119567, 35.33352588067079125, -2.999999999999971578 ) ) ;
#14922 = EDGE_CURVE ( 'NONE', #18686, #7232, #21749, .T. ) ;
#14923 = CARTESIAN_POINT ( 'NONE',  ( 18.03138881840328978, 11.33611194795357946, -60.11697748794928486 ) ) ;
#14924 = VERTEX_POINT ( 'NONE', #4340 ) ;
#14925 = EDGE_LOOP ( 'NONE', ( #4529, #10085, #3701, #18270 ) ) ;
#14926 = AXIS2_PLACEMENT_3D ( 'NONE', #18529, #21555, #4447 ) ;
#14927 = ORIENTED_EDGE ( 'NONE', *, *, #1518, .T. ) ;
#14928 = ORIENTED_EDGE ( 'NONE', *, *, #6337, .T. ) ;
#14929 = CARTESIAN_POINT ( 'NONE',  ( 2.999999999999998224, 22.00000000000000000, 6.485281374238567764 ) ) ;
#14930 = AXIS2_PLACEMENT_3D ( 'NONE', #10750, #21091, #17638 ) ;
#14931 = CARTESIAN_POINT ( 'NONE',  ( -24.99999999999999645, 20.00000000000000000, 25.00000000000001421 ) ) ;
#14932 = ORIENTED_EDGE ( 'NONE', *, *, #20868, .T. ) ;
#14933 = DIRECTION ( 'NONE',  ( 1.000000000000000000, 0.000000000000000000, 0.000000000000000000 ) ) ;
#14934 = CARTESIAN_POINT ( 'NONE',  ( -0.9710767271268349043, 13.15819026053459240, 6.949333411110965919 ) ) ;
#14935 = ORIENTED_EDGE ( 'NONE', *, *, #21938, .T. ) ;
#14936 = AXIS2_PLACEMENT_3D ( 'NONE', #8296, #20665, #10001 ) ;
#14937 = CARTESIAN_POINT ( 'NONE',  ( -28.52469787935782364, 10.00000000000000000, 4.095854054471899985 ) ) ;
#14938 = CARTESIAN_POINT ( 'NONE',  ( 47.83731665821556334, 10.00000000000000000, -38.93845529828706020 ) ) ;
#14939 = DIRECTION ( 'NONE',  ( -0.000000000000000000, 1.000000000000000000, -0.000000000000000000 ) ) ;
#14940 = CARTESIAN_POINT ( 'NONE',  ( -35.00000000000000000, 40.00000000000000000, 1.387778780781445676E-14 ) ) ;
#14941 = CARTESIAN_POINT ( 'NONE',  ( 2.775557561562891351E-14, 2.775557561562891351E-14, 5.750000000000001776 ) ) ;
#14942 = EDGE_CURVE ( 'NONE', #4779, #8231, #14829, .T. ) ;
#14943 = EDGE_CURVE ( 'NONE', #14743, #14562, #16581, .T. ) ;
#14944 = AXIS2_PLACEMENT_3D ( 'NONE', #18306, #5585, #16475 ) ;
#14945 = CIRCLE ( 'NONE', #22291, 6.499999999999999112 ) ;
#14946 = CARTESIAN_POINT ( 'NONE',  ( 2.220446049250313081E-13, -2.498001805406602216E-13, -6.859353255829918616 ) ) ;
#14947 = EDGE_CURVE ( 'NONE', #3371, #384, #10067, .T. ) ;
#14948 = CARTESIAN_POINT ( 'NONE',  ( -47.83731665821552781, 10.00000000000000000, -38.93845529828706731 ) ) ;
#14949 = AXIS2_PLACEMENT_3D ( 'NONE', #6210, #11242, #18121 ) ;
#14950 = VERTEX_POINT ( 'NONE', #3411 ) ;
#14951 = VERTEX_POINT ( 'NONE', #1224 ) ;
#14952 = ORIENTED_EDGE ( 'NONE', *, *, #20842, .F. ) ;
#14953 = CARTESIAN_POINT ( 'NONE',  ( -22.40268525210710848, 21.30540434957256934, 58.66274428449824541 ) ) ;
#14954 = DIRECTION ( 'NONE',  ( -0.000000000000000000, -0.000000000000000000, 1.000000000000000000 ) ) ;
#14955 = MECHANICAL_DESIGN_GEOMETRIC_PRESENTATION_REPRESENTATION (  '', ( #13126 ), #3995 ) ;
#14956 = DIRECTION ( 'NONE',  ( -1.000000000000000000, 1.296372316667914327E-16, 0.000000000000000000 ) ) ;
#14957 = FACE_OUTER_BOUND ( 'NONE', #21060, .T. ) ;
#14958 = CARTESIAN_POINT ( 'NONE',  ( 33.51030287062395274, 15.12081897056660651, 2.800654218530485018 ) ) ;
#14959 = DIRECTION ( 'NONE',  ( 0.000000000000000000, 0.000000000000000000, 1.000000000000000000 ) ) ;
#14960 = CARTESIAN_POINT ( 'NONE',  ( 0.7810292038143733517, 39.98537128388858264, 49.65442669227650896 ) ) ;
#14961 = CARTESIAN_POINT ( 'NONE',  ( -6.450211378059112377, 39.75599570130062688, -53.02618257463311835 ) ) ;
#14962 = DIRECTION ( 'NONE',  ( -0.000000000000000000, 1.000000000000000000, -0.000000000000000000 ) ) ;
#14963 = ORIENTED_EDGE ( 'NONE', *, *, #20547, .T. ) ;
#14964 = DIRECTION ( 'NONE',  ( 0.000000000000000000, 0.000000000000000000, -1.000000000000000000 ) ) ;
#14965 = DIRECTION ( 'NONE',  ( 0.000000000000000000, 0.000000000000000000, 1.000000000000000000 ) ) ;
#14966 = DIRECTION ( 'NONE',  ( -1.000000000000000000, 0.000000000000000000, 0.000000000000000000 ) ) ;
#14967 = LINE ( 'NONE', #7767, #7835 ) ;
#14968 = ORIENTED_EDGE ( 'NONE', *, *, #9112, .T. ) ;
#14969 = B_SPLINE_CURVE_WITH_KNOTS ( 'NONE', 3,
 ( #13184, #11602, #11488, #10091 ),
 .UNSPECIFIED., .F., .F.,
 ( 4, 4 ),
 ( 0.000000000000000000, 0.0005662878734225370485 ),
 .UNSPECIFIED. ) ;
#14970 = ORIENTED_EDGE ( 'NONE', *, *, #9562, .F. ) ;
#14971 = AXIS2_PLACEMENT_3D ( 'NONE', #2513, #13020, #2272 ) ;
#14972 = DIRECTION ( 'NONE',  ( 0.000000000000000000, 0.000000000000000000, 1.000000000000000000 ) ) ;
#14973 = DIRECTION ( 'NONE',  ( 0.000000000000000000, 0.000000000000000000, 1.000000000000000000 ) ) ;
#14974 = EDGE_CURVE ( 'NONE', #10123, #16148, #15185, .T. ) ;
#14975 = CARTESIAN_POINT ( 'NONE',  ( 16.56444186175109934, -26.79308242454903066, 3.000000000000023537 ) ) ;
#14976 = CIRCLE ( 'NONE', #21219, 60.00000000000000000 ) ;
#14977 = ADVANCED_FACE ( 'NONE', ( #6848 ), #10151, .F. ) ;
#14978 = CARTESIAN_POINT ( 'NONE',  ( 8.105735169339924440, 40.00000000000001421, -53.00649291450380929 ) ) ;
#14979 = ORIENTED_EDGE ( 'NONE', *, *, #19076, .F. ) ;
#14980 = ADVANCED_FACE ( 'NONE', ( #11876, #13690 ), #20707, .T. ) ;
#14981 = EDGE_CURVE ( 'NONE', #5071, #2772, #5017, .T. ) ;
#14982 = DIRECTION ( 'NONE',  ( 0.000000000000000000, -0.000000000000000000, 1.000000000000000000 ) ) ;
#14983 = AXIS2_PLACEMENT_3D ( 'NONE', #21619, #14494, #5685 ) ;
#14984 = CARTESIAN_POINT ( 'NONE',  ( 0.000000000000000000, 30.00000000000000000, 0.000000000000000000 ) ) ;
#14985 = CARTESIAN_POINT ( 'NONE',  ( -2.580942297915963746, 40.00000000000000000, 50.31086577932750714 ) ) ;
#14986 = DIRECTION ( 'NONE',  ( 6.505213034913038160E-19, 3.903127820947822896E-18, 1.000000000000000000 ) ) ;
#14987 = CARTESIAN_POINT ( 'NONE',  ( -12.68897045256290745, 28.00829229206842186, -44.74667050109236754 ) ) ;
#14988 = CARTESIAN_POINT ( 'NONE',  ( 31.92986134326236680, -18.22261011550291343, -2.800654218530485018 ) ) ;
#14989 = EDGE_LOOP ( 'NONE', ( #13864, #10558, #11068, #1306 ) ) ;
#14990 = CARTESIAN_POINT ( 'NONE',  ( 35.00000000000001421, 5.000000000000000000, 1.540743955509788682E-30 ) ) ;
#14991 = DIRECTION ( 'NONE',  ( -0.000000000000000000, -1.000000000000000000, -0.000000000000000000 ) ) ;
#14992 = LINE ( 'NONE', #7491, #9136 ) ;
#14993 = CARTESIAN_POINT ( 'NONE',  ( 5.999999999999998224, -20.00000000000000000, -5.999999999999999112 ) ) ;
#14994 = CARTESIAN_POINT ( 'NONE',  ( -0.05198106984670706338, 39.99998426957630926, -48.77439678740044116 ) ) ;
#14995 = ORIENTED_EDGE ( 'NONE', *, *, #7865, .F. ) ;
#14996 = APPLICATION_CONTEXT ( 'automotive_design' ) ;
#14997 = AXIS2_PLACEMENT_3D ( 'NONE', #9141, #17959, #17846 ) ;
#14998 = EDGE_CURVE ( 'NONE', #3151, #6360, #7151, .T. ) ;
#14999 = DIRECTION ( 'NONE',  ( 0.000000000000000000, 0.000000000000000000, 1.000000000000000000 ) ) ;
#15000 = CARTESIAN_POINT ( 'NONE',  ( 4.936596639065399472, 31.11077005834403408, 2.999999999999995559 ) ) ;
#15001 = EDGE_CURVE ( 'NONE', #1314, #5420, #1298, .T. ) ;
#15002 = ORIENTED_EDGE ( 'NONE', *, *, #16145, .T. ) ;
#15003 = ORIENTED_EDGE ( 'NONE', *, *, #12523, .T. ) ;
#15004 =( NAMED_UNIT ( * ) SI_UNIT ( $, .STERADIAN. ) SOLID_ANGLE_UNIT ( ) );
#15005 = ORIENTED_EDGE ( 'NONE', *, *, #16452, .T. ) ;
#15006 = CARTESIAN_POINT ( 'NONE',  ( 19.99999999999998579, 20.00000000000000711, -60.62177826491069510 ) ) ;
#15007 = ADVANCED_FACE ( 'NONE', ( #10266 ), #11998, .T. ) ;
#15008 = DIRECTION ( 'NONE',  ( -0.4332438415859278247, 0.000000000000000000, -0.9012767464701768594 ) ) ;
#15009 = VECTOR ( 'NONE', #6695, 1000.000000000000000 ) ;
#15010 = CARTESIAN_POINT ( 'NONE',  ( -42.50000000000000711, -12.00000000000000000, 47.50000000000000711 ) ) ;
#15011 = CARTESIAN_POINT ( 'NONE',  ( 12.92329681834241484, 4.659497110088489435, 58.43073491095716321 ) ) ;
#15012 = CYLINDRICAL_SURFACE ( 'NONE', #9078, 1.000000000000000888 ) ;
#15013 = ORIENTED_EDGE ( 'NONE', *, *, #17180, .F. ) ;
#15014 = DIRECTION ( 'NONE',  ( -0.000000000000000000, -1.000000000000000000, -0.000000000000000000 ) ) ;
#15015 = CARTESIAN_POINT ( 'NONE',  ( 34.99999999999980815, 39.97500000000000142, 52.49999999999922551 ) ) ;
#15016 = VERTEX_POINT ( 'NONE', #13468 ) ;
#15017 = DIRECTION ( 'NONE',  ( 0.000000000000000000, 0.000000000000000000, 1.000000000000000000 ) ) ;
#15018 = CARTESIAN_POINT ( 'NONE',  ( -15.00000000000001421, 20.00000000000000000, -45.82575694955838230 ) ) ;
#15019 = DIRECTION ( 'NONE',  ( 8.659560562354892183E-17, 0.7071067811865507924, -0.7071067811865441310 ) ) ;
#15020 = CARTESIAN_POINT ( 'NONE',  ( -42.50000000000000711, -9.600000000000001421, -47.50000000000000000 ) ) ;
#15021 = ORIENTED_EDGE ( 'NONE', *, *, #9333, .F. ) ;
#15022 = DIRECTION ( 'NONE',  ( 0.000000000000000000, 0.000000000000000000, 1.000000000000000000 ) ) ;
#15023 = CARTESIAN_POINT ( 'NONE',  ( 0.1539325450101303450, 40.00000000000000000, -48.91834387730068556 ) ) ;
#15024 = VERTEX_POINT ( 'NONE', #6614 ) ;
#15025 = FACE_OUTER_BOUND ( 'NONE', #21767, .T. ) ;
#15026 =( LENGTH_UNIT ( ) NAMED_UNIT ( * ) SI_UNIT ( .MILLI., .METRE. ) );
#15027 = VERTEX_POINT ( 'NONE', #17256 ) ;
#15028 = ADVANCED_FACE ( 'NONE', ( #4792 ), #8744, .T. ) ;
#15029 = CARTESIAN_POINT ( 'NONE',  ( 14.30947201678935699, 34.00909065833927514, 56.34794761833577326 ) ) ;
#15030 = CARTESIAN_POINT ( 'NONE',  ( -21.97438720605733664, 22.98755168577401520, -2.999999999999971578 ) ) ;
#15031 = CARTESIAN_POINT ( 'NONE',  ( 15.62385314663624669, 32.51590977305029639, -59.38867318806720164 ) ) ;
#15032 = ADVANCED_FACE ( 'NONE', ( #8671 ), #17368, .F. ) ;
#15033 = ORIENTED_EDGE ( 'NONE', *, *, #9583, .F. ) ;
#15034 = VERTEX_POINT ( 'NONE', #18876 ) ;
#15035 = ORIENTED_EDGE ( 'NONE', *, *, #21645, .T. ) ;
#15036 = ORIENTED_EDGE ( 'NONE', *, *, #2752, .F. ) ;
#15037 = DIRECTION ( 'NONE',  ( -1.000000000000000000, -1.208970125616077665E-17, 0.000000000000000000 ) ) ;
#15038 = DIRECTION ( 'NONE',  ( -0.000000000000000000, -1.000000000000000000, -0.000000000000000000 ) ) ;
#15039 = VECTOR ( 'NONE', #8853, 1000.000000000000000 ) ;
#15040 = CIRCLE ( 'NONE', #16133, 19.11328065563151668 ) ;
#15041 = EDGE_CURVE ( 'NONE', #2190, #7646, #1343, .T. ) ;
#15042 = EDGE_LOOP ( 'NONE', ( #3300, #19518, #1848, #17380 ) ) ;
#15043 = CARTESIAN_POINT ( 'NONE',  ( -29.36548507648009831, -13.83143812983123055, 2.999999999999995559 ) ) ;
#15044 = CARTESIAN_POINT ( 'NONE',  ( 0.3890599824573822696, 12.99957889865121174, 7.000138250717951927 ) ) ;
#15045 = ORIENTED_EDGE ( 'NONE', *, *, #20076, .T. ) ;
#15046 = LINE ( 'NONE', #15277, #16487 ) ;
#15047 = CARTESIAN_POINT ( 'NONE',  ( 42.50000000000000711, -11.97499999999999964, 47.50000000000000711 ) ) ;
#15048 = ORIENTED_EDGE ( 'NONE', *, *, #20012, .T. ) ;
#15049 = CARTESIAN_POINT ( 'NONE',  ( -2.995584608082024758, -1.237002266245722515, -50.27666343020536743 ) ) ;
#15050 = EDGE_CURVE ( 'NONE', #4972, #2875, #21062, .T. ) ;
#15051 = CARTESIAN_POINT ( 'NONE',  ( 2.775557561562891351E-14, -2.775557561562891351E-14, 2.999999999999999112 ) ) ;
#15052 = FACE_OUTER_BOUND ( 'NONE', #3815, .T. ) ;
#15053 = CARTESIAN_POINT ( 'NONE',  ( -9.144347024359422704, 37.80953375799288807, -56.77060857467738231 ) ) ;
#15054 = EDGE_CURVE ( 'NONE', #10705, #10746, #7296, .T. ) ;
#15055 = AXIS2_PLACEMENT_3D ( 'NONE', #1677, #19327, #17246 ) ;
#15056 = DIRECTION ( 'NONE',  ( -1.000000000000000000, -1.815202222194849261E-15, 0.000000000000000000 ) ) ;
#15057 = ORIENTED_EDGE ( 'NONE', *, *, #2741, .T. ) ;
#15058 = ORIENTED_EDGE ( 'NONE', *, *, #1553, .T. ) ;
#15059 = EDGE_CURVE ( 'NONE', #22419, #13252, #12996, .T. ) ;
#15060 = VERTEX_POINT ( 'NONE', #5564 ) ;
#15061 = CARTESIAN_POINT ( 'NONE',  ( -16.25447798254661791, 8.309829536803846395, 57.03340146943939004 ) ) ;
#15062 = DIRECTION ( 'NONE',  ( 1.266830946243004623E-16, -1.000000000000000000, -3.903127820947817503E-18 ) ) ;
#15063 = DIRECTION ( 'NONE',  ( 1.000000000000000000, 0.000000000000000000, 0.000000000000000000 ) ) ;
#15064 = FACE_OUTER_BOUND ( 'NONE', #21175, .T. ) ;
#15065 = VECTOR ( 'NONE', #5312, 1000.000000000000000 ) ;
#15066 = CARTESIAN_POINT ( 'NONE',  ( 35.00000000000000000, 39.00000000000000711, 4.258610482196280173E-15 ) ) ;
#15067 = EDGE_CURVE ( 'NONE', #6177, #10749, #15866, .T. ) ;
#15068 = ORIENTED_EDGE ( 'NONE', *, *, #7889, .T. ) ;
#15069 = CARTESIAN_POINT ( 'NONE',  ( 4.918774254216024211, -31.11359284679388182, 2.999999999999995559 ) ) ;
#15070 = DIRECTION ( 'NONE',  ( -6.505213034913038160E-19, -3.903127820947822896E-18, -1.000000000000000000 ) ) ;
#15071 = DIRECTION ( 'NONE',  ( -0.000000000000000000, -1.000000000000000000, -0.000000000000000000 ) ) ;
#15072 = CARTESIAN_POINT ( 'NONE',  ( -0.6290164960522119930, 40.00000000000000000, -49.48738346577703595 ) ) ;
#15073 = ORIENTED_EDGE ( 'NONE', *, *, #356, .T. ) ;
#15074 = CARTESIAN_POINT ( 'NONE',  ( 3.330669073875469621E-13, -1.110223024625156540E-13, -2.999999999999971578 ) ) ;
#15075 = DIRECTION ( 'NONE',  ( 0.000000000000000000, 1.000000000000000000, 0.000000000000000000 ) ) ;
#15076 = FACE_BOUND ( 'NONE', #22062, .T. ) ;
#15077 = ORIENTED_EDGE ( 'NONE', *, *, #15968, .T. ) ;
#15078 = DIRECTION ( 'NONE',  ( 0.000000000000000000, 1.000000000000000000, 0.000000000000000000 ) ) ;
#15079 = DIRECTION ( 'NONE',  ( 0.000000000000000000, -1.000000000000000000, 0.000000000000000000 ) ) ;
#15080 = FACE_OUTER_BOUND ( 'NONE', #22316, .T. ) ;
#15081 = DIRECTION ( 'NONE',  ( 0.000000000000000000, 0.000000000000000000, -1.000000000000000000 ) ) ;
#15082 = EDGE_LOOP ( 'NONE', ( #17491, #5335, #12110, #17294, #1762, #10232 ) ) ;
#15083 = VECTOR ( 'NONE', #9852, 1000.000000000000114 ) ;
#15084 = CIRCLE ( 'NONE', #16195, 34.90673715956759082 ) ;
#15085 = EDGE_CURVE ( 'NONE', #548, #19255, #9006, .T. ) ;
#15086 = ORIENTED_EDGE ( 'NONE', *, *, #16037, .T. ) ;
#15087 = CARTESIAN_POINT ( 'NONE',  ( -3.328561921038571736, -3.140496874697064733, 49.62333327021501361 ) ) ;
#15088 = DIRECTION ( 'NONE',  ( 1.000000000000000000, 0.000000000000000000, 0.000000000000000000 ) ) ;
#15089 = ORIENTED_EDGE ( 'NONE', *, *, #3224, .T. ) ;
#15090 = DIRECTION ( 'NONE',  ( 0.000000000000000000, -0.000000000000000000, 1.000000000000000000 ) ) ;
#15091 = EDGE_CURVE ( 'NONE', #21392, #5486, #21435, .T. ) ;
#15092 = CARTESIAN_POINT ( 'NONE',  ( 5.275737522157127195E-15, 12.49999999999999645, 0.000000000000000000 ) ) ;
#15093 = CARTESIAN_POINT ( 'NONE',  ( -1.387778780781445518E-14, 20.00000000000000355, -105.0000000000000142 ) ) ;
#15094 = CARTESIAN_POINT ( 'NONE',  ( 17.99999999999998579, 20.00000000000000355, 102.0000000000000142 ) ) ;
#15095 = DIRECTION ( 'NONE',  ( -0.000000000000000000, 1.000000000000000000, -0.000000000000000000 ) ) ;
#15096 = AXIS2_PLACEMENT_3D ( 'NONE', #2237, #630, #11162 ) ;
#15097 = CARTESIAN_POINT ( 'NONE',  ( -35.99819890246936893, 7.463862311150981199, -1.999999999999984457 ) ) ;
#15098 = VERTEX_POINT ( 'NONE', #1809 ) ;
#15099 = CARTESIAN_POINT ( 'NONE',  ( 14.99999999999998579, 20.38555233723673155, 45.82575694955838941 ) ) ;
#15100 = CARTESIAN_POINT ( 'NONE',  ( 2.995584608080545053, -1.237002266245787130, 50.27666343020442241 ) ) ;
#15101 = AXIS2_PLACEMENT_3D ( 'NONE', #433, #9385, #670 ) ;
#15102 = DIRECTION ( 'NONE',  ( 0.000000000000000000, 0.000000000000000000, 1.000000000000000000 ) ) ;
#15103 = CARTESIAN_POINT ( 'NONE',  ( -0.06361866581498207274, 39.99997619040497909, -48.78343476366760001 ) ) ;
#15104 = AXIS2_PLACEMENT_3D ( 'NONE', #20895, #5412, #13641 ) ;
#15105 = EDGE_CURVE ( 'NONE', #8849, #312, #10807, .T. ) ;
#15106 = VERTEX_POINT ( 'NONE', #3647 ) ;
#15107 = DIRECTION ( 'NONE',  ( -1.000000000000000000, 0.000000000000000000, 0.000000000000000000 ) ) ;
#15108 = CARTESIAN_POINT ( 'NONE',  ( -21.41958700883257904, -27.56232195404059837, -2.999999999999992450 ) ) ;
#15109 = EDGE_CURVE ( 'NONE', #16547, #14672, #15763, .T. ) ;
#15110 =( BOUNDED_SURFACE ( )  B_SPLINE_SURFACE ( 3, 2, ( 
 ( #17653, #14430, #21439 ),
 ( #21324, #5742, #4042 ),
 ( #10648, #21215, #14200 ),
 ( #5965, #5861, #19497 ),
 ( #11010, #12936, #19947 ),
 ( #2301, #1963, #3802 ) ),
 .UNSPECIFIED., .F., .F., .F. ) 
 B_SPLINE_SURFACE_WITH_KNOTS ( ( 4, 2, 4 ),
 ( 3, 3 ),
 ( 0.000000000000000000, 0.002858401832365848987, 0.005716803664731697973 ),
 ( 0.000000000000000000, 1.000000000000000000 ),
 .UNSPECIFIED. ) 
 GEOMETRIC_REPRESENTATION_ITEM ( )  RATIONAL_B_SPLINE_SURFACE ( (
 ( 1.000000000000000000, 0.7200096751079149149, 1.000000000000000000),
 ( 1.000000000000000000, 0.7065285139740180576, 1.000000000000000000),
 ( 1.000000000000000000, 0.6920701670995640375, 1.000000000000000000),
 ( 1.000000000000000000, 0.6615687397052482099, 1.000000000000000000),
 ( 1.000000000000000000, 0.6455195629506302879, 1.000000000000000000),
 ( 1.000000000000000000, 0.6290213284793395587, 1.000000000000000000) ) ) 
 REPRESENTATION_ITEM ( '' )  SURFACE ( )  );
#15111 = CIRCLE ( 'NONE', #11841, 3.999999999999994671 ) ;
#15112 = EDGE_LOOP ( 'NONE', ( #12276, #5182, #10103, #22444 ) ) ;
#15113 = CIRCLE ( 'NONE', #5265, 2.499999999999998668 ) ;
#15114 = EDGE_LOOP ( 'NONE', ( #21993, #2235 ) ) ;
#15115 = AXIS2_PLACEMENT_3D ( 'NONE', #436, #14520, #21301 ) ;
#15116 = CARTESIAN_POINT ( 'NONE',  ( 118.3444743520637985, 176.9080996817152425, -11.76735212958570642 ) ) ;
#15117 = ORIENTED_EDGE ( 'NONE', *, *, #9619, .F. ) ;
#15118 = CARTESIAN_POINT ( 'NONE',  ( 11.06593724743305529, 40.00000000000000000, 53.99256019164672438 ) ) ;
#15119 = DIRECTION ( 'NONE',  ( -6.505213034913038160E-19, -3.903127820947822896E-18, -1.000000000000000000 ) ) ;
#15120 = CARTESIAN_POINT ( 'NONE',  ( -27.56232195404058416, 21.41958700883256483, 2.999999999999995559 ) ) ;
#15121 = LINE ( 'NONE', #19484, #1753 ) ;
#15122 = CARTESIAN_POINT ( 'NONE',  ( 2.601474714586665016, 5.225049111783174105, -39.07471001004994093 ) ) ;
#15123 = EDGE_LOOP ( 'NONE', ( #11929, #5216 ) ) ;
#15124 = CARTESIAN_POINT ( 'NONE',  ( -42.50000000000000711, -12.00000000000000000, -47.50000000000000000 ) ) ;
#15125 = DIRECTION ( 'NONE',  ( -0.000000000000000000, -1.000000000000000000, -0.000000000000000000 ) ) ;
#15126 = VERTEX_POINT ( 'NONE', #21499 ) ;
#15127 = CARTESIAN_POINT ( 'NONE',  ( 2.775557561562891351E-14, -2.775557561562891351E-14, 2.999999999999999112 ) ) ;
#15128 = CARTESIAN_POINT ( 'NONE',  ( -34.99999999999997868, 0.000000000000000000, 54.99999999999698730 ) ) ;
#15129 = DIRECTION ( 'NONE',  ( 0.000000000000000000, 0.000000000000000000, -1.000000000000000000 ) ) ;
#15130 = CIRCLE ( 'NONE', #5278, 36.76383501243555685 ) ;
#15131 = CARTESIAN_POINT ( 'NONE',  ( 9.952189117650823036, 40.00000000000000000, 53.64426396172073197 ) ) ;
#15132 = ORIENTED_EDGE ( 'NONE', *, *, #18548, .T. ) ;
#15133 = CARTESIAN_POINT ( 'NONE',  ( -5.651049805244181101, 39.99999999999999289, -51.93203809155826889 ) ) ;
#15134 = ORIENTED_EDGE ( 'NONE', *, *, #11384, .F. ) ;
#15135 = DIRECTION ( 'NONE',  ( 6.505213034913038160E-19, 3.903127820947822896E-18, 1.000000000000000000 ) ) ;
#15136 = EDGE_CURVE ( 'NONE', #19883, #1691, #14471, .T. ) ;
#15137 = ORIENTED_EDGE ( 'NONE', *, *, #6352, .T. ) ;
#15138 = DIRECTION ( 'NONE',  ( 0.000000000000000000, -1.000000000000000000, 0.000000000000000000 ) ) ;
#15139 = AXIS2_PLACEMENT_3D ( 'NONE', #1239, #1358, #15428 ) ;
#15140 = CARTESIAN_POINT ( 'NONE',  ( -28.07080038625073115, -14.29266125237904639, -2.999999999999981792 ) ) ;
#15141 = DIRECTION ( 'NONE',  ( 0.1421319796954317316, 0.000000000000000000, 0.9898477157360406897 ) ) ;
#15142 = VECTOR ( 'NONE', #11903, 1000.000000000000000 ) ;
#15143 = CARTESIAN_POINT ( 'NONE',  ( 22.20813536596259041, 23.24072130216428178, -58.62062866457824128 ) ) ;
#15144 = ORIENTED_EDGE ( 'NONE', *, *, #4213, .T. ) ;
#15145 = EDGE_LOOP ( 'NONE', ( #19208, #22538 ) ) ;
#15146 = AXIS2_PLACEMENT_3D ( 'NONE', #4039, #18104, #8943 ) ;
#15147 = VERTEX_POINT ( 'NONE', #16101 ) ;
#15148 = EDGE_LOOP ( 'NONE', ( #16911, #11494, #21712, #1643, #9863, #11737 ) ) ;
#15149 = CARTESIAN_POINT ( 'NONE',  ( 0.7837852459090882684, 24.89976299354472289, 6.967910395774115528 ) ) ;
#15150 = AXIS2_PLACEMENT_3D ( 'NONE', #18083, #9391, #16365 ) ;
#15151 = DIRECTION ( 'NONE',  ( -1.000000000000000000, -9.002681209562840861E-16, 0.000000000000000000 ) ) ;
#15152 = ADVANCED_FACE ( 'NONE', ( #17488 ), #5353, .F. ) ;
#15153 = ORIENTED_EDGE ( 'NONE', *, *, #11296, .F. ) ;
#15154 = CARTESIAN_POINT ( 'NONE',  ( -13.00000000000000178, 20.00000000000000000, -11.32475165290611407 ) ) ;
#15155 = CARTESIAN_POINT ( 'NONE',  ( 18.00000000000035882, -2.752196816394091375E-14, -4.999999999999997335 ) ) ;
#15156 = ORIENTED_EDGE ( 'NONE', *, *, #815, .F. ) ;
#15157 = FACE_OUTER_BOUND ( 'NONE', #21960, .T. ) ;
#15158 = CARTESIAN_POINT ( 'NONE',  ( 21.41958700883261812, 27.56232195404056995, -2.999999999999995559 ) ) ;
#15159 = ORIENTED_EDGE ( 'NONE', *, *, #5747, .T. ) ;
#15160 = DIRECTION ( 'NONE',  ( -1.000000000000000000, 0.000000000000000000, 0.000000000000000000 ) ) ;
#15161 = CARTESIAN_POINT ( 'NONE',  ( -17.09029715894913437, 27.64365646977270785, 3.000000000000012879 ) ) ;
#15162 = EDGE_CURVE ( 'NONE', #20565, #14456, #1266, .T. ) ;
#15163 = CARTESIAN_POINT ( 'NONE',  ( 28.88846368933370456, 19.59430950039303809, -2.999999999999975131 ) ) ;
#15164 = CARTESIAN_POINT ( 'NONE',  ( -0.09368727804205789766, 39.99996055794411376, 48.80679978730719881 ) ) ;
#15165 = AXIS2_PLACEMENT_3D ( 'NONE', #8497, #15471, #15129 ) ;
#15166 = FACE_OUTER_BOUND ( 'NONE', #18381, .T. ) ;
#15167 = ORIENTED_EDGE ( 'NONE', *, *, #12938, .T. ) ;
#15168 = ORIENTED_EDGE ( 'NONE', *, *, #12349, .F. ) ;
#15169 = CIRCLE ( 'NONE', #20682, 22.00000000000000000 ) ;
#15170 = VERTEX_POINT ( 'NONE', #10827 ) ;
#15171 = CARTESIAN_POINT ( 'NONE',  ( -18.34034842040193425, 28.02508533843026939, 60.20240101110111652 ) ) ;
#15172 = FACE_OUTER_BOUND ( 'NONE', #21334, .T. ) ;
#15173 = VECTOR ( 'NONE', #16844, 1000.000000000000000 ) ;
#15174 = ADVANCED_FACE ( 'NONE', ( #299 ), #10444, .T. ) ;
#15175 = CARTESIAN_POINT ( 'NONE',  ( -15.34286839272958147, 7.164559734098759236, -59.29291272740923091 ) ) ;
#15176 = CYLINDRICAL_SURFACE ( 'NONE', #5995, 0.9999999999999956701 ) ;
#15177 = VECTOR ( 'NONE', #9882, 1000.000000000000000 ) ;
#15178 = CYLINDRICAL_SURFACE ( 'NONE', #20359, 36.76383501243555685 ) ;
#15179 = ORIENTED_EDGE ( 'NONE', *, *, #21113, .F. ) ;
#15180 = PLANE ( 'NONE',  #12033 ) ;
#15181 = CARTESIAN_POINT ( 'NONE',  ( -4.110274091176338018, 39.99999999999999289, -51.15360534159206196 ) ) ;
#15182 = EDGE_CURVE ( 'NONE', #2957, #18735, #14141, .T. ) ;
#15183 = CYLINDRICAL_SURFACE ( 'NONE', #16000, 19.11328065563150957 ) ;
#15184 = EDGE_CURVE ( 'NONE', #8848, #21260, #177, .T. ) ;
#15185 = LINE ( 'NONE', #6728, #22547 ) ;
#15186 = ORIENTED_EDGE ( 'NONE', *, *, #3317, .F. ) ;
#15187 = CARTESIAN_POINT ( 'NONE',  ( -10.35284963923112933, 39.23826485901322769, 54.78050591838192673 ) ) ;
#15188 = CARTESIAN_POINT ( 'NONE',  ( 15.03694978697417994, 3.237610724645296312, 56.60357944353837922 ) ) ;
#15189 = CIRCLE ( 'NONE', #15551, 14.00000000000000000 ) ;
#15190 = ADVANCED_FACE ( 'NONE', ( #5682 ), #16312, .F. ) ;
#15191 = AXIS2_PLACEMENT_3D ( 'NONE', #16559, #21848, #13325 ) ;
#15192 = ORIENTED_EDGE ( 'NONE', *, *, #7210, .T. ) ;
#15193 = AXIS2_PLACEMENT_3D ( 'NONE', #21968, #4090, #9806 ) ;
#15194 = DIRECTION ( 'NONE',  ( -6.505213034913038160E-19, -3.903127820947822896E-18, -1.000000000000000000 ) ) ;
#15195 = CARTESIAN_POINT ( 'NONE',  ( -35.00000000000000000, 2.142135623730931471, 1.387778780781445676E-14 ) ) ;
#15196 = DIRECTION ( 'NONE',  ( 0.000000000000000000, 0.000000000000000000, 1.000000000000000000 ) ) ;
#15197 = ADVANCED_FACE ( 'NONE', ( #524 ), #4986, .F. ) ;
#15198 = AXIS2_PLACEMENT_3D ( 'NONE', #1722, #7325, #8706 ) ;
#15199 = B_SPLINE_CURVE_WITH_KNOTS ( 'NONE', 3,
 ( #9591, #9490, #9373, #6166, #2618, #22092, #11076, #16470, #7654, #18409 ),
 .UNSPECIFIED., .F., .F.,
 ( 4, 2, 2, 2, 4 ),
 ( 0.000000000000000000, 0.0006732693119717972395, 0.001346538623943594479, 0.002019807935915391827, 0.002693077247887188958 ),
 .UNSPECIFIED. ) ;
#15200 = ORIENTED_EDGE ( 'NONE', *, *, #1802, .T. ) ;
#15201 = CONICAL_SURFACE ( 'NONE', #17025, 2.525000000000110489, 0.7853981633971014453 ) ;
#15202 = EDGE_LOOP ( 'NONE', ( #5872, #2854, #737, #5784 ) ) ;
#15203 = CARTESIAN_POINT ( 'NONE',  ( 0.1895185485179805007, -3.154272558796861858, 47.17695316422283014 ) ) ;
#15204 = CARTESIAN_POINT ( 'NONE',  ( 35.00000000000000000, 17.00000000000000000, 39.00000000000003553 ) ) ;
#15205 = VECTOR ( 'NONE', #20705, 1000.000000000000000 ) ;
#15206 = VECTOR ( 'NONE', #12385, 1000.000000000000000 ) ;
#15207 = EDGE_LOOP ( 'NONE', ( #8637, #3512, #22540, #20586 ) ) ;
#15208 = B_SPLINE_CURVE_WITH_KNOTS ( 'NONE', 3,
 ( #12392, #1415, #6793, #20657 ),
 .UNSPECIFIED., .F., .F.,
 ( 4, 4 ),
 ( 9.715086429499893182E-07, 0.001929643240674650765 ),
 .UNSPECIFIED. ) ;
#15209 = AXIS2_PLACEMENT_3D ( 'NONE', #17739, #7092, #10292 ) ;
#15210 = CARTESIAN_POINT ( 'NONE',  ( 48.93401015228426587, 10.00000000000000000, 46.57614213197968667 ) ) ;
#15211 = DIRECTION ( 'NONE',  ( -6.505213034913038160E-19, -3.903127820947822896E-18, -1.000000000000000000 ) ) ;
#15212 = DIRECTION ( 'NONE',  ( -1.000000000000000000, 0.000000000000000000, 0.000000000000000000 ) ) ;
#15213 = CARTESIAN_POINT ( 'NONE',  ( -20.11656324090263936, 10.00164725896635076, -58.12608834080167952 ) ) ;
#15214 = DIRECTION ( 'NONE',  ( -0.000000000000000000, -1.000000000000000000, -0.000000000000000000 ) ) ;
#15215 = AXIS2_PLACEMENT_3D ( 'NONE', #10742, #17747, #9043 ) ;
#15216 = DIRECTION ( 'NONE',  ( 0.000000000000000000, 0.000000000000000000, -1.000000000000000000 ) ) ;
#15217 = VERTEX_POINT ( 'NONE', #17942 ) ;
#15218 = CARTESIAN_POINT ( 'NONE',  ( 9.855264211176363531, 31.32970427768387722, 43.22210574525158933 ) ) ;
#15219 = FACE_OUTER_BOUND ( 'NONE', #7051, .T. ) ;
#15220 = DIRECTION ( 'NONE',  ( -1.000000000000000000, 0.000000000000000000, 0.000000000000000000 ) ) ;
#15221 = CARTESIAN_POINT ( 'NONE',  ( -35.92356703407480012, -4.104166344909336850, 2.932460736555823733 ) ) ;
#15222 = EDGE_CURVE ( 'NONE', #21941, #15452, #16306, .T. ) ;
#15223 = ORIENTED_EDGE ( 'NONE', *, *, #22619, .T. ) ;
#15224 = EDGE_CURVE ( 'NONE', #21131, #5874, #18147, .T. ) ;
#15225 = CARTESIAN_POINT ( 'NONE',  ( -34.74700806321090596, 12.00937115242645170, 2.800654218530481465 ) ) ;
#15226 = CARTESIAN_POINT ( 'NONE',  ( 5.833333333333339255, 6.180730040185842711, 40.61164310337068173 ) ) ;
#15227 = AXIS2_PLACEMENT_3D ( 'NONE', #13496, #11686, #20511 ) ;
#15228 = EDGE_CURVE ( 'NONE', #15404, #2168, #19246, .T. ) ;
#15229 = ORIENTED_EDGE ( 'NONE', *, *, #17462, .F. ) ;
#15230 = AXIS2_PLACEMENT_3D ( 'NONE', #19114, #10381, #17379 ) ;
#15231 = VERTEX_POINT ( 'NONE', #14610 ) ;
#15232 = ORIENTED_EDGE ( 'NONE', *, *, #22535, .T. ) ;
#15233 = DIRECTION ( 'NONE',  ( -0.000000000000000000, 1.000000000000000000, -0.000000000000000000 ) ) ;
#15234 = CARTESIAN_POINT ( 'NONE',  ( 35.00000000000000000, 10.00000000000000000, 2.365113165210053967E-14 ) ) ;
#15235 = CARTESIAN_POINT ( 'NONE',  ( 2.775557561562891351E-14, -2.775557561562891351E-14, 2.999999999999999112 ) ) ;
#15236 = CARTESIAN_POINT ( 'NONE',  ( 22.26748298433281548, -22.28024240313505899, 2.999999999999995559 ) ) ;
#15237 = DIRECTION ( 'NONE',  ( -1.000000000000000000, 0.000000000000000000, 0.000000000000000000 ) ) ;
#15238 = AXIS2_PLACEMENT_3D ( 'NONE', #16527, #11371, #14904 ) ;
#15239 = ORIENTED_EDGE ( 'NONE', *, *, #19588, .F. ) ;
#15240 = CARTESIAN_POINT ( 'NONE',  ( -3.418729828831206752E-14, -1.500000000000015099, 15.99999999999970512 ) ) ;
#15241 = DIRECTION ( 'NONE',  ( 0.000000000000000000, 0.000000000000000000, 1.000000000000000000 ) ) ;
#15242 = ORIENTED_EDGE ( 'NONE', *, *, #7371, .F. ) ;
#15243 = CARTESIAN_POINT ( 'NONE',  ( -15.00000000000001599, 19.61444766276327556, -45.82575694955838230 ) ) ;
#15244 = AXIS2_PLACEMENT_3D ( 'NONE', #8559, #13815, #18026 ) ;
#15245 = CARTESIAN_POINT ( 'NONE',  ( -35.00000000000000000, 17.00000000000000000, 2.365113165210053967E-14 ) ) ;
#15246 = EDGE_CURVE ( 'NONE', #22344, #3930, #13360, .T. ) ;
#15247 = DIRECTION ( 'NONE',  ( -6.505213034913038160E-19, -3.903127820947822896E-18, -1.000000000000000000 ) ) ;
#15248 = CARTESIAN_POINT ( 'NONE',  ( 6.913287910056896912, 40.00000000000000711, 52.51234321215227396 ) ) ;
#15249 = VERTEX_POINT ( 'NONE', #21726 ) ;
#15250 = DIRECTION ( 'NONE',  ( 0.000000000000000000, 1.000000000000000000, -0.000000000000000000 ) ) ;
#15251 = ORIENTED_EDGE ( 'NONE', *, *, #22148, .F. ) ;
#15252 = DIRECTION ( 'NONE',  ( -1.000000000000000000, -1.208970125616046080E-17, 6.505213034913038160E-19 ) ) ;
#15253 = CARTESIAN_POINT ( 'NONE',  ( -19.51193873661508960, 31.10741194645162366, 57.96703944061304270 ) ) ;
#15254 = ORIENTED_EDGE ( 'NONE', *, *, #6804, .T. ) ;
#15255 = DIRECTION ( 'NONE',  ( 0.000000000000000000, 1.000000000000000000, 0.000000000000000000 ) ) ;
#15256 = CARTESIAN_POINT ( 'NONE',  ( -42.49999999999996447, 7.000000000000000000, -50.00000000000000711 ) ) ;
#15257 = CARTESIAN_POINT ( 'NONE',  ( 34.99999999999980815, 26.00000000000000355, 54.99999999999922551 ) ) ;
#15258 = B_SPLINE_CURVE_WITH_KNOTS ( 'NONE', 3,
 ( #9802, #8419, #1097, #6358, #1198, #15389 ),
 .UNSPECIFIED., .F., .F.,
 ( 4, 2, 4 ),
 ( 1.939479807224432123E-18, 0.002694896630593770787, 0.005389793261187539840 ),
 .UNSPECIFIED. ) ;
#15259 = TOROIDAL_SURFACE ( 'NONE', #5389, 50.00000000000000000, 10.00000000000000000 ) ;
#15260 = CARTESIAN_POINT ( 'NONE',  ( 18.14868794606629265, 11.58103667096281875, -57.62894917896122138 ) ) ;
#15261 = CIRCLE ( 'NONE', #8341, 27.99999999999999645 ) ;
#15262 = CIRCLE ( 'NONE', #10882, 0.9999999999999974465 ) ;
#15263 = EDGE_LOOP ( 'NONE', ( #3938, #21688, #8208, #17954, #13783, #5536, #1013, #19118, #482, #18667, #16488, #8138 ) ) ;
#15264 = ORIENTED_EDGE ( 'NONE', *, *, #6055, .T. ) ;
#15265 = ORIENTED_EDGE ( 'NONE', *, *, #17589, .T. ) ;
#15266 =( NAMED_UNIT ( * ) SI_UNIT ( $, .STERADIAN. ) SOLID_ANGLE_UNIT ( ) );
#15267 = EDGE_CURVE ( 'NONE', #13925, #5266, #22543, .T. ) ;
#15268 = ORIENTED_EDGE ( 'NONE', *, *, #7467, .T. ) ;
#15269 = CARTESIAN_POINT ( 'NONE',  ( 21.41958700883261812, 27.56232195404056995, -2.999999999999995559 ) ) ;
#15270 = DIRECTION ( 'NONE',  ( 1.000000000000000000, 0.000000000000000000, 0.000000000000000000 ) ) ;
#15271 = CIRCLE ( 'NONE', #8335, 6.499999999999999112 ) ;
#15272 = AXIS2_PLACEMENT_3D ( 'NONE', #19512, #9426, #14217 ) ;
#15273 = ORIENTED_EDGE ( 'NONE', *, *, #1472, .F. ) ;
#15274 = DIRECTION ( 'NONE',  ( -6.505213034913038160E-19, -3.903127820947822896E-18, -1.000000000000000000 ) ) ;
#15275 = CARTESIAN_POINT ( 'NONE',  ( 0.000000000000000000, 30.00000000000000000, 0.000000000000000000 ) ) ;
#15276 = ORIENTED_EDGE ( 'NONE', *, *, #11635, .F. ) ;
#15277 = CARTESIAN_POINT ( 'NONE',  ( -2.347663744114242057, -31.41239365194231681, -6.999999999999950262 ) ) ;
#15278 = AXIS2_PLACEMENT_3D ( 'NONE', #12587, #16382, #12819 ) ;
#15279 = ORIENTED_EDGE ( 'NONE', *, *, #11396, .F. ) ;
#15280 = DIRECTION ( 'NONE',  ( -0.000000000000000000, 1.000000000000000000, -0.000000000000000000 ) ) ;
#15281 = AXIS2_PLACEMENT_3D ( 'NONE', #15306, #20706, #20375 ) ;
#15282 = CARTESIAN_POINT ( 'NONE',  ( 32.83234229683737482, -11.85401191286897316, -2.999999999999971578 ) ) ;
#15283 = DIRECTION ( 'NONE',  ( -6.505213034913038160E-19, -3.903127820947822896E-18, -1.000000000000000000 ) ) ;
#15284 = CARTESIAN_POINT ( 'NONE',  ( -36.54278193890295512, -4.025500340002762911, -2.800654218530457484 ) ) ;
#15285 = CARTESIAN_POINT ( 'NONE',  ( -8.759110511859015347, 7.803016162472652617, 42.56552456877081170 ) ) ;
#15286 = ADVANCED_FACE ( 'NONE', ( #2597 ), #12880, .T. ) ;
#15287 = TOROIDAL_SURFACE ( 'NONE', #22638, 34.90673715956759082, 8.750000000000000000 ) ;
#15288 = VERTEX_POINT ( 'NONE', #20127 ) ;
#15289 = TOROIDAL_SURFACE ( 'NONE', #18234, 34.90673715956759082, 8.750000000000000000 ) ;
#15290 = ORIENTED_EDGE ( 'NONE', *, *, #13287, .T. ) ;
#15291 = CIRCLE ( 'NONE', #17857, 31.50000000000001421 ) ;
#15292 = ORIENTED_EDGE ( 'NONE', *, *, #2035, .T. ) ;
#15293 = EDGE_CURVE ( 'NONE', #2580, #16652, #17778, .T. ) ;
#15294 = CIRCLE ( 'NONE', #6532, 34.90673715956759082 ) ;
#15295 = ORIENTED_EDGE ( 'NONE', *, *, #2659, .T. ) ;
#15296 = CARTESIAN_POINT ( 'NONE',  ( -18.97285531159713301, 26.38757670764340446, 60.36948798341369127 ) ) ;
#15297 = CARTESIAN_POINT ( 'NONE',  ( 3.608224830031758756E-13, -2.775557561562891351E-14, -4.999999999999997335 ) ) ;
#15298 = B_SPLINE_SURFACE_WITH_KNOTS ( 'NONE', 1, 3, ( 
 ( #16876, #9657, #16646, #18479, #951, #13413, #7947, #1074, #15133, #8279, #8063, #22038, #4747, #1287, #11716, #18712, #3017, #19278, #17546, #5402 ),
 ( #15706, #8394, #8500, #12056, #17427, #12383, #6907, #1856, #22494, #10542, #1746, #7115, #13868, #20887, #22384, #15366, #15810, #6673, #19163, #1628 ) ),
 .UNSPECIFIED., .F., .F., .F.,
 ( 2, 2 ),
 ( 4, 2, 2, 2, 2, 2, 2, 2, 2, 4 ),
 ( 0.000000000000000000, 1.000000000000000000 ),
 ( 0.000000000000000000, 0.002777081680065593070, 0.004165622520098389604, 0.005554163360131186139, 0.006942704200163982674, 0.008331245040196779209, 0.009025515460213177910, 0.009719785880229574876, 0.01041405630024597358, 0.01110832672026237228 ),
 .UNSPECIFIED. ) ;
#15299 = CARTESIAN_POINT ( 'NONE',  ( -36.06598984771569860, 10.00000000000000000, -48.42385786802031333 ) ) ;
#15300 = CARTESIAN_POINT ( 'NONE',  ( 6.692425168897880638, 39.70962082636729917, 53.18141012597577344 ) ) ;
#15301 = DIRECTION ( 'NONE',  ( 1.000000000000000000, 0.000000000000000000, -0.000000000000000000 ) ) ;
#15302 = AXIS2_PLACEMENT_3D ( 'NONE', #1458, #8331, #15304 ) ;
#15303 = EDGE_LOOP ( 'NONE', ( #9276, #16464, #18434, #5191 ) ) ;
#15304 = DIRECTION ( 'NONE',  ( 0.000000000000000000, 0.000000000000000000, 1.000000000000000000 ) ) ;
#15305 = CARTESIAN_POINT ( 'NONE',  ( -6.286720893520962861, 40.00000000000000711, -52.22859683420058730 ) ) ;
#15306 = CARTESIAN_POINT ( 'NONE',  ( -22.97438720605751783, 22.98755168577401520, 3.000000000000023537 ) ) ;
#15307 = CARTESIAN_POINT ( 'NONE',  ( -4.918774254215691144, 31.11359284679385340, -7.000000000000006217 ) ) ;
#15308 = VERTEX_POINT ( 'NONE', #18173 ) ;
#15309 = DIRECTION ( 'NONE',  ( 0.000000000000000000, -0.7071067811867928210, -0.7071067811863022134 ) ) ;
#15310 = CIRCLE ( 'NONE', #5452, 33.99999999999999289 ) ;
#15311 = ORIENTED_EDGE ( 'NONE', *, *, #3202, .T. ) ;
#15312 = CARTESIAN_POINT ( 'NONE',  ( -35.00000000000058265, 28.00000000000000000, -52.90000000000076597 ) ) ;
#15313 = EDGE_CURVE ( 'NONE', #22096, #18746, #2771, .T. ) ;
#15314 = CARTESIAN_POINT ( 'NONE',  ( 7.776554266669417956E-15, -4.648749848372173865, -45.43309249825056639 ) ) ;
#15315 = FACE_BOUND ( 'NONE', #8957, .T. ) ;
#15316 = ORIENTED_EDGE ( 'NONE', *, *, #5012, .T. ) ;
#15317 = AXIS2_PLACEMENT_3D ( 'NONE', #21343, #14571, #21582 ) ;
#15318 = EDGE_CURVE ( 'NONE', #15629, #2277, #11525, .T. ) ;
#15319 = EDGE_CURVE ( 'NONE', #3734, #4131, #10818, .T. ) ;
#15320 = ORIENTED_EDGE ( 'NONE', *, *, #10957, .T. ) ;
#15321 = CARTESIAN_POINT ( 'NONE',  ( -7.688876120686208182, -2.941163814652081321, 52.37456181060783678 ) ) ;
#15322 = DIRECTION ( 'NONE',  ( -6.505213034913038160E-19, -3.903127820947822896E-18, -1.000000000000000000 ) ) ;
#15323 = ORIENTED_EDGE ( 'NONE', *, *, #3552, .T. ) ;
#15324 = FACE_OUTER_BOUND ( 'NONE', #7307, .T. ) ;
#15325 = EDGE_CURVE ( 'NONE', #10226, #15849, #15555, .T. ) ;
#15326 = DIRECTION ( 'NONE',  ( -0.000000000000000000, -0.000000000000000000, 1.000000000000000000 ) ) ;
#15327 = CARTESIAN_POINT ( 'NONE',  ( 35.00000000000058265, 40.00000000000000000, -57.10000000000076170 ) ) ;
#15328 = CARTESIAN_POINT ( 'NONE',  ( -17.96644252022830912, 11.16803817567492807, -57.57522208103581818 ) ) ;
#15329 = B_SPLINE_CURVE_WITH_KNOTS ( 'NONE', 3,
 ( #21187, #21299, #5589, #19580, #786, #16122, #19919, #21639, #434, #4009, #6173, #16241, #9258, #7545, #18416, #20038, #5936, #551 ),
 .UNSPECIFIED., .F., .F.,
 ( 4, 2, 2, 2, 2, 2, 2, 2, 4 ),
 ( 0.000000000000000000, 0.001465012583164687458, 0.002930025166329374917, 0.004395037749494062375, 0.005860050332658749833, 0.008790075498988123015, 0.01025508808215280787, 0.01098759437373514510, 0.01172010066531747885 ),
 .UNSPECIFIED. ) ;
#15330 = CARTESIAN_POINT ( 'NONE',  ( -7.033428926742907983, 33.31269054942710284, -41.47353357286036157 ) ) ;
#15331 = EDGE_CURVE ( 'NONE', #5289, #938, #8259, .T. ) ;
#15332 = CARTESIAN_POINT ( 'NONE',  ( -11.88509939556638351, 36.18356491088834304, 55.39957109942756119 ) ) ;
#15333=STYLED_ITEM('',(#22748),#18090);
#15334 = ORIENTED_EDGE ( 'NONE', *, *, #20251, .F. ) ;
#15335 = CARTESIAN_POINT ( 'NONE',  ( 42.50000000000000711, -12.00000000000000000, 47.50000000000000711 ) ) ;
#15336 = FACE_BOUND ( 'NONE', #20875, .T. ) ;
#15337 = FACE_OUTER_BOUND ( 'NONE', #5433, .T. ) ;
#15338 = DIRECTION ( 'NONE',  ( -0.000000000000000000, -1.000000000000000000, -0.000000000000000000 ) ) ;
#15339 = ORIENTED_EDGE ( 'NONE', *, *, #21626, .T. ) ;
#15340 = EDGE_CURVE ( 'NONE', #20510, #14603, #6365, .T. ) ;
#15341 = DIRECTION ( 'NONE',  ( 0.000000000000000000, 0.000000000000000000, -1.000000000000000000 ) ) ;
#15342 = CARTESIAN_POINT ( 'NONE',  ( 4.106440533746705590, 5.536968433055398542, 39.55567250430844695 ) ) ;
#15343 = CIRCLE ( 'NONE', #3306, 36.76383501243555685 ) ;
#15344 = EDGE_LOOP ( 'NONE', ( #10377, #14860 ) ) ;
#15345 = AXIS2_PLACEMENT_3D ( 'NONE', #9474, #9233, #16456 ) ;
#15346 = ORIENTED_EDGE ( 'NONE', *, *, #9129, .F. ) ;
#15347 = SHAPE_DEFINITION_REPRESENTATION ( #4380, #21420 ) ;
#15348 = EDGE_CURVE ( 'NONE', #13123, #3413, #18505, .T. ) ;
#15349 = ORIENTED_EDGE ( 'NONE', *, *, #504, .F. ) ;
#15350 = DIRECTION ( 'NONE',  ( -1.000000000000000000, 7.725943281265459575E-14, 0.000000000000000000 ) ) ;
#15351 = CARTESIAN_POINT ( 'NONE',  ( -0.1963897509097776439, -3.154216256273198571, 47.17168727994772581 ) ) ;
#15352 = CARTESIAN_POINT ( 'NONE',  ( 34.00000000000000000, 6.180736333215571143, 4.163799117100999770E-15 ) ) ;
#15353 = EDGE_CURVE ( 'NONE', #9680, #6332, #8096, .T. ) ;
#15354 = CARTESIAN_POINT ( 'NONE',  ( 17.38288706075490353, 10.07729229769341828, 59.93358289200956790 ) ) ;
#15355 = DIRECTION ( 'NONE',  ( 0.000000000000000000, 0.000000000000000000, -1.000000000000000000 ) ) ;
#15356 = ORIENTED_EDGE ( 'NONE', *, *, #3537, .F. ) ;
#15357 = FACE_OUTER_BOUND ( 'NONE', #10961, .T. ) ;
#15358 = CARTESIAN_POINT ( 'NONE',  ( 10.39230484541308819, -1.500000000000015099, 6.000000000000008882 ) ) ;
#15359 = ORIENTED_EDGE ( 'NONE', *, *, #145, .T. ) ;
#15360 = DIRECTION ( 'NONE',  ( -0.000000000000000000, -0.000000000000000000, 1.000000000000000000 ) ) ;
#15361 = DIRECTION ( 'NONE',  ( 0.000000000000000000, 0.000000000000000000, 1.000000000000000000 ) ) ;
#15363 = AXIS2_PLACEMENT_3D ( 'NONE', #3907, #3570, #1946 ) ;
#15362 = DIRECTION ( 'NONE',  ( -1.000000000000000000, 0.000000000000000000, -0.000000000000000000 ) ) ;
#15364 = DIRECTION ( 'NONE',  ( 6.505213034913038160E-19, 3.903127820947822896E-18, 1.000000000000000000 ) ) ;
#15365 = VERTEX_POINT ( 'NONE', #7635 ) ;
#15366 = CARTESIAN_POINT ( 'NONE',  ( -8.555717074797012600, 39.50215801696872830, -54.09939910646557593 ) ) ;
#15367 = ADVANCED_FACE ( 'NONE', ( #15052 ), #2484, .T. ) ;
#15368 = VERTEX_POINT ( 'NONE', #16453 ) ;
#15369 = DIRECTION ( 'NONE',  ( -1.000000000000000000, 0.000000000000000000, 0.000000000000000000 ) ) ;
#15370 = CARTESIAN_POINT ( 'NONE',  ( -32.09841355225970005, 5.093313992686226754, 2.999999999999995559 ) ) ;
#15371 = ORIENTED_EDGE ( 'NONE', *, *, #8448, .T. ) ;
#15372 = CARTESIAN_POINT ( 'NONE',  ( -25.00000000000000000, 20.00000000000000000, 6.487780019669002523E-15 ) ) ;
#15373 = DIRECTION ( 'NONE',  ( 0.000000000000000000, 0.000000000000000000, 1.000000000000000000 ) ) ;
#15374 = CARTESIAN_POINT ( 'NONE',  ( -1.387778780781445676E-14, 20.00000000000000000, 98.00000000000000000 ) ) ;
#15375 = CARTESIAN_POINT ( 'NONE',  ( 17.76087593031624579, 33.76750075041049826, -57.47290953699885563 ) ) ;
#15376 = ORIENTED_EDGE ( 'NONE', *, *, #22339, .T. ) ;
#15377 = CIRCLE ( 'NONE', #9158, 22.00000000000000000 ) ;
#15378 = VERTEX_POINT ( 'NONE', #11405 ) ;
#15379 = ORIENTED_EDGE ( 'NONE', *, *, #15600, .T. ) ;
#15380 = ADVANCED_FACE ( 'NONE', ( #2711 ), #761, .F. ) ;
#15381 = ORIENTED_EDGE ( 'NONE', *, *, #6152, .F. ) ;
#15382 = CARTESIAN_POINT ( 'NONE',  ( -2.979639132232873688, 22.39635031597078907, 6.492556366683235325 ) ) ;
#15383 = LINE ( 'NONE', #19068, #5606 ) ;
#15384 = DIRECTION ( 'NONE',  ( 0.000000000000000000, 0.000000000000000000, -1.000000000000000000 ) ) ;
#15385 = VERTEX_POINT ( 'NONE', #3159 ) ;
#15386 = DIRECTION ( 'NONE',  ( 1.296372316667914327E-16, 1.000000000000000000, -0.000000000000000000 ) ) ;
#15387 = FACE_OUTER_BOUND ( 'NONE', #18375, .T. ) ;
#15388 = EDGE_LOOP ( 'NONE', ( #8150, #12388, #20327, #19968 ) ) ;
#15389 = CARTESIAN_POINT ( 'NONE',  ( 9.103081159015154356, 0.03030367950454006254, 53.87333532811640424 ) ) ;
#15390 = ORIENTED_EDGE ( 'NONE', *, *, #15990, .T. ) ;
#15391 = CARTESIAN_POINT ( 'NONE',  ( 35.16985127952398926, 10.70799354677376414, -2.000000000000001776 ) ) ;
#15392 = CARTESIAN_POINT ( 'NONE',  ( -26.50842683089750551, 24.41514043009179602, -7.000000000000006217 ) ) ;
#15393 = DIRECTION ( 'NONE',  ( 0.000000000000000000, 0.000000000000000000, 1.000000000000000000 ) ) ;
#15394 = CARTESIAN_POINT ( 'NONE',  ( -1.328644774245273830, 39.98974582701344360, 49.74044376501583997 ) ) ;
#15395 = AXIS2_PLACEMENT_3D ( 'NONE', #15724, #1653, #17448 ) ;
#15396 = DIRECTION ( 'NONE',  ( -0.000000000000000000, 1.000000000000000000, -0.000000000000000000 ) ) ;
#15397 = EDGE_CURVE ( 'NONE', #18218, #15664, #13718, .T. ) ;
#15398 = CARTESIAN_POINT ( 'NONE',  ( -17.99999999999963762, -2.576882599977457532E-14, -4.999999999999997335 ) ) ;
#15399 = EDGE_LOOP ( 'NONE', ( #12934, #13744, #3566, #13565, #19923 ) ) ;
#15400 = EDGE_CURVE ( 'NONE', #2388, #1875, #1319, .T. ) ;
#15401 = AXIS2_PLACEMENT_3D ( 'NONE', #6552, #4494, #9971 ) ;
#15402 = ORIENTED_EDGE ( 'NONE', *, *, #469, .T. ) ;
#15403 = ORIENTED_EDGE ( 'NONE', *, *, #4272, .T. ) ;
#15404 = VERTEX_POINT ( 'NONE', #15622 ) ;
#15405 = CARTESIAN_POINT ( 'NONE',  ( -13.56354382738803288, 2.142135623730931471, 56.03997097393687454 ) ) ;
#15406 = CARTESIAN_POINT ( 'NONE',  ( -13.00000000000011546, 42.51666049839536043, 60.00099999999999767 ) ) ;
#15407 = CYLINDRICAL_SURFACE ( 'NONE', #8344, 25.00000000000000711 ) ;
#15408 = CARTESIAN_POINT ( 'NONE',  ( 6.877234547883836591, 39.69228528355510832, 53.28061374633059444 ) ) ;
#15409 = B_SPLINE_CURVE_WITH_KNOTS ( 'NONE', 3,
 ( #10714, #1916, #8897, #15873 ),
 .UNSPECIFIED., .F., .F.,
 ( 4, 4 ),
 ( 0.001875451646902967593, 0.003761979286331313191 ),
 .UNSPECIFIED. ) ;
#15410 = ORIENTED_EDGE ( 'NONE', *, *, #21649, .T. ) ;
#15411 = DIRECTION ( 'NONE',  ( 0.000000000000000000, 0.000000000000000000, -1.000000000000000000 ) ) ;
#15412 = DIRECTION ( 'NONE',  ( 0.000000000000000000, 0.000000000000000000, 1.000000000000000000 ) ) ;
#15413 = CARTESIAN_POINT ( 'NONE',  ( 2.602085213965210642E-15, 7.999999999999994671, 0.000000000000000000 ) ) ;
#15414 = DIRECTION ( 'NONE',  ( 1.000000000000000000, 1.208970125616045926E-17, 0.000000000000000000 ) ) ;
#15415 = SURFACE_STYLE_FILL_AREA ( #19000 ) ;
#15416 = AXIS2_PLACEMENT_3D ( 'NONE', #9190, #19409, #3711 ) ;
#15417 = ORIENTED_EDGE ( 'NONE', *, *, #171, .T. ) ;
#15418 = CARTESIAN_POINT ( 'NONE',  ( 1.734723475976807094E-14, 20.00000000000000000, 70.71067811865476926 ) ) ;
#15419 = EDGE_CURVE ( 'NONE', #20378, #4759, #6997, .T. ) ;
#15420 = ORIENTED_EDGE ( 'NONE', *, *, #16979, .F. ) ;
#15421 = CARTESIAN_POINT ( 'NONE',  ( -25.00000000000000000, -20.00000000000000000, 6.487780019669002523E-15 ) ) ;
#15422 = CYLINDRICAL_SURFACE ( 'NONE', #9691, 2.099999999999997868 ) ;
#15423 = CARTESIAN_POINT ( 'NONE',  ( -35.00000000000000000, 10.00000000000000000, 41.00000000000002132 ) ) ;
#15424 = ORIENTED_EDGE ( 'NONE', *, *, #15510, .F. ) ;
#15425 = EDGE_CURVE ( 'NONE', #10311, #13677, #6595, .T. ) ;
#15426 = ORIENTED_EDGE ( 'NONE', *, *, #3932, .T. ) ;
#15427 = APPLICATION_CONTEXT ( 'automotive_design' ) ;
#15428 = DIRECTION ( 'NONE',  ( 0.000000000000000000, 0.000000000000000000, 1.000000000000000000 ) ) ;
#15429 = CIRCLE ( 'NONE', #19845, 6.499999999999999112 ) ;
#15430 = CYLINDRICAL_SURFACE ( 'NONE', #2485, 6.499999999999999112 ) ;
#15431 = ORIENTED_EDGE ( 'NONE', *, *, #18035, .F. ) ;
#15432 = CARTESIAN_POINT ( 'NONE',  ( 13.76792553423402232, 13.99810558461763321, 45.26963775109940258 ) ) ;
#15433 = EDGE_CURVE ( 'NONE', #21019, #15288, #19305, .T. ) ;
#15434 = CARTESIAN_POINT ( 'NONE',  ( 41.39271818392635538, 7.000000000000000000, 5.943569790512533757 ) ) ;
#15435 = CARTESIAN_POINT ( 'NONE',  ( -30.07487443287951123, 12.31876324338268525, 3.000000000000023537 ) ) ;
#15436 = CARTESIAN_POINT ( 'NONE',  ( -22.35494499951317948, 21.77768233190463576, -58.65240855008566712 ) ) ;
#15437 = CARTESIAN_POINT ( 'NONE',  ( -2.636016739579310375, 39.95887900714455299, 50.67500335283390456 ) ) ;
#15438 = CARTESIAN_POINT ( 'NONE',  ( -11.59291124596518863, 39.24500985576617040, 55.27372209264447633 ) ) ;
#15439 = ORIENTED_EDGE ( 'NONE', *, *, #20302, .T. ) ;
#15440 = CARTESIAN_POINT ( 'NONE',  ( 10.38220159744132864, 30.85082733156616186, 43.52345836121337186 ) ) ;
#15441 = DIRECTION ( 'NONE',  ( 0.000000000000000000, -0.000000000000000000, 1.000000000000000000 ) ) ;
#15442 = DIRECTION ( 'NONE',  ( 0.000000000000000000, 1.000000000000000000, 0.000000000000000000 ) ) ;
#15443 = EDGE_CURVE ( 'NONE', #3845, #10716, #9913, .T. ) ;
#15444 = EDGE_CURVE ( 'NONE', #13122, #1817, #4807, .T. ) ;
#15445 = DIRECTION ( 'NONE',  ( 1.000000000000000000, 0.000000000000000000, 0.000000000000000000 ) ) ;
#15446 = CIRCLE ( 'NONE', #1562, 0.9999999999999974465 ) ;
#15447 = VERTEX_POINT ( 'NONE', #3046 ) ;
#15448 = CARTESIAN_POINT ( 'NONE',  ( 1.368200027493404197E-14, -0.6657802223429165611, -48.32248901598325119 ) ) ;
#15449 = FACE_OUTER_BOUND ( 'NONE', #8052, .T. ) ;
#15450 = CIRCLE ( 'NONE', #18393, 1.000000000000000888 ) ;
#15451 = ADVANCED_FACE ( 'NONE', ( #8310 ), #7906, .T. ) ;
#15452 = VERTEX_POINT ( 'NONE', #10346 ) ;
#15453 = EDGE_CURVE ( 'NONE', #18082, #1931, #7163, .T. ) ;
#15454 = SHAPE_DEFINITION_REPRESENTATION ( #21955, #10907 ) ;
#15455 = ORIENTED_EDGE ( 'NONE', *, *, #20926, .F. ) ;
#15456 = CARTESIAN_POINT ( 'NONE',  ( 42.50000000000000711, -5.000000000000000000, -47.50000000000000000 ) ) ;
#15457 = DIRECTION ( 'NONE',  ( 6.505213034913038160E-19, 3.903127820947822896E-18, 1.000000000000000000 ) ) ;
#15458 = CARTESIAN_POINT ( 'NONE',  ( -35.00000000000000000, 0.000000000000000000, 1.387778780781445676E-14 ) ) ;
#15459 = CIRCLE ( 'NONE', #8886, 10.00000000000000000 ) ;
#15460 = CYLINDRICAL_SURFACE ( 'NONE', #12698, 19.99999999999999289 ) ;
#15461 = EDGE_CURVE ( 'NONE', #2202, #16547, #11551, .T. ) ;
#15462 = DIRECTION ( 'NONE',  ( 0.000000000000000000, -0.7071067811865500152, -0.7071067811865451302 ) ) ;
#15463 = ORIENTED_EDGE ( 'NONE', *, *, #6306, .T. ) ;
#15464 = CARTESIAN_POINT ( 'NONE',  ( 6.696867368503558448E-15, 40.00000000000000000, 39.73397172404483513 ) ) ;
#15465 = VECTOR ( 'NONE', #5588, 1000.000000000000000 ) ;
#15466 = CARTESIAN_POINT ( 'NONE',  ( -1.423424233832598640, -32.35999952201590446, -2.999999999999971578 ) ) ;
#15467 = EDGE_LOOP ( 'NONE', ( #4865, #16711 ) ) ;
#15468 = CARTESIAN_POINT ( 'NONE',  ( 9.377138775076085508, -4.928932188134512948, -51.00555535510811467 ) ) ;
#15469 = VECTOR ( 'NONE', #19743, 1000.000000000000000 ) ;
#15470 = CARTESIAN_POINT ( 'NONE',  ( 9.103081159019511759, 0.03030367950604059835, -53.87333532811884851 ) ) ;
#15471 = DIRECTION ( 'NONE',  ( -0.000000000000000000, -1.000000000000000000, -0.000000000000000000 ) ) ;
#15472 = CARTESIAN_POINT ( 'NONE',  ( 7.262748859126449297, 39.65386577974343396, 53.48190593274512139 ) ) ;
#15473 = VERTEX_POINT ( 'NONE', #4774 ) ;
#15474 = LINE ( 'NONE', #12164, #4914 ) ;
#15475 = EDGE_LOOP ( 'NONE', ( #1065, #11469, #19086, #224 ) ) ;
#15476 = CYLINDRICAL_SURFACE ( 'NONE', #608, 6.499999999999999112 ) ;
#15477 = EDGE_CURVE ( 'NONE', #12921, #14751, #1679, .T. ) ;
#15478 = LINE ( 'NONE', #19054, #21391 ) ;
#15479 = ORIENTED_EDGE ( 'NONE', *, *, #17683, .F. ) ;
#15480 = CARTESIAN_POINT ( 'NONE',  ( 12.99999999999993960, 42.51666049839543149, -105.0010000000000048 ) ) ;
#15481 = CARTESIAN_POINT ( 'NONE',  ( -10.27431133777641215, -4.928932188134511172, -51.43682631505697600 ) ) ;
#15482 = DIRECTION ( 'NONE',  ( -6.505213034913038160E-19, -3.903127820947822896E-18, -1.000000000000000000 ) ) ;
#15483 = EDGE_CURVE ( 'NONE', #3496, #10039, #15933, .T. ) ;
#15484 = CIRCLE ( 'NONE', #18056, 2.000000000000001776 ) ;
#15485 = DIRECTION ( 'NONE',  ( 0.000000000000000000, 0.000000000000000000, 1.000000000000000000 ) ) ;
#15486 = EDGE_CURVE ( 'NONE', #19594, #20460, #3872, .T. ) ;
#15487 = AXIS2_PLACEMENT_3D ( 'NONE', #6878, #6761, #13499 ) ;
#15488 = ORIENTED_EDGE ( 'NONE', *, *, #6797, .F. ) ;
#15489 = ORIENTED_EDGE ( 'NONE', *, *, #9510, .F. ) ;
#15490 = ORIENTED_EDGE ( 'NONE', *, *, #730, .F. ) ;
#15491 = DIRECTION ( 'NONE',  ( 0.000000000000000000, 0.000000000000000000, 1.000000000000000000 ) ) ;
#15492 = EDGE_LOOP ( 'NONE', ( #1108, #19279, #4610, #12094 ) ) ;
#15493 = DIRECTION ( 'NONE',  ( 6.505213034913038160E-19, 3.903127820947822896E-18, 1.000000000000000000 ) ) ;
#15494 = CARTESIAN_POINT ( 'NONE',  ( 22.29010897948492698, 17.41268129326155645, 58.63841251601399307 ) ) ;
#15495 = AXIS2_PLACEMENT_3D ( 'NONE', #19678, #5918, #14499 ) ;
#15496 = CARTESIAN_POINT ( 'NONE',  ( 7.549845394205005000, 39.99999999999999289, -52.78128352898642106 ) ) ;
#15497 = ORIENTED_EDGE ( 'NONE', *, *, #21239, .F. ) ;
#15498 = CARTESIAN_POINT ( 'NONE',  ( -34.99999999999999289, 0.000000000000000000, 4.999999999999969802 ) ) ;
#15499 = DIRECTION ( 'NONE',  ( 1.000000000000000000, 0.000000000000000000, 0.000000000000000000 ) ) ;
#15500 = VERTEX_POINT ( 'NONE', #4992 ) ;
#15501 = AXIS2_PLACEMENT_3D ( 'NONE', #12894, #14839, #21396 ) ;
#15502 = FACE_OUTER_BOUND ( 'NONE', #8216, .T. ) ;
#15503 = ORIENTED_EDGE ( 'NONE', *, *, #13136, .F. ) ;
#15504 = DIRECTION ( 'NONE',  ( 1.296372316667914327E-16, 1.000000000000000000, -0.000000000000000000 ) ) ;
#15505 = CARTESIAN_POINT ( 'NONE',  ( 34.74700806321118307, -12.00937115242653519, -2.800654218530457484 ) ) ;
#15506 = CARTESIAN_POINT ( 'NONE',  ( 30.13956425491259949, 21.05198877411795877, -2.800654218530485018 ) ) ;
#15507 = CARTESIAN_POINT ( 'NONE',  ( -9.177444842293963845, 39.41890427424159782, 54.36989715539939283 ) ) ;
#15508=STYLED_ITEM('',(#22727),#10654);
#15509 = LINE ( 'NONE', #8534, #19142 ) ;
#15510 = EDGE_CURVE ( 'NONE', #5004, #5574, #10076, .T. ) ;
#15511 = CARTESIAN_POINT ( 'NONE',  ( 10.70799354677381920, -35.16985127952404611, -2.800654218530477912 ) ) ;
#15512 = EDGE_LOOP ( 'NONE', ( #8569, #18021, #14039, #1885, #4071, #21147, #11328, #6741, #16461, #7928, #684, #20315, #18916, #16067, #6486, #12317, #6930, #8257, #13449, #11305, #18277, #20133, #16414, #3814, #7884, #4169, #17631, #8278, #16631, #15708, #20487, #2554, #16223, #16207, #21642, #17420, #20336, #2086, #7126, #22596, #9018, #8092, #10250, #19956, #20674, #11370, #9553, #3247, #12119, #15972, #3108, #12014, #10294, #15251, #3451, #4550, #12826, #18342, #12728, #22146, #21117, #8732, #18805, #8710, #4317, #18478, #4175, #21128, #3543, #6465, #21342, #17285, #15153, #11999, #2707, #17442, #6947, #13662, #11791, #13452, #1410, #7966, #5641, #7037, #20417, #14692, #618, #17782, #11860, #13600, #19771, #1229, #12201, #9998, #19850, #20538, #9138, #8352, #15905, #5727, #16946, #11147, #9175, #3777, #16658, #6781, #19207, #17375, #5123, #17519, #21459, #827, #2584, #20772, #13908, #2282, #16374, #21878, #15356, #21395, #21832, #13910, #19387, #9858, #19396, #5151, #14412, #9188, #795, #20442, #6346 ) ) ;
#15513 = ORIENTED_EDGE ( 'NONE', *, *, #16230, .T. ) ;
#15514 = ADVANCED_FACE ( 'NONE', ( #1547 ), #10440, .T. ) ;
#15515 = VERTEX_POINT ( 'NONE', #1664 ) ;
#15516 = CIRCLE ( 'NONE', #9685, 1.000000000000000888 ) ;
#15517 = ORIENTED_EDGE ( 'NONE', *, *, #2163, .T. ) ;
#15518 = CARTESIAN_POINT ( 'NONE',  ( 42.50000000000000711, -12.00000000000000000, 41.00000000000000711 ) ) ;
#15519 = CARTESIAN_POINT ( 'NONE',  ( -11.93772187171643040, -33.46652738560690921, -2.999999999999999112 ) ) ;
#15520 = CARTESIAN_POINT ( 'NONE',  ( -9.952189117650851458, 40.00000000000000000, -53.64426396172072486 ) ) ;
#15521 = DIRECTION ( 'NONE',  ( -1.000000000000000000, 0.000000000000000000, 0.000000000000000000 ) ) ;
#15522 = CARTESIAN_POINT ( 'NONE',  ( 6.646840102370911829, 39.71385755071619172, 53.15684333213135204 ) ) ;
#15523 = ORIENTED_EDGE ( 'NONE', *, *, #21829, .T. ) ;
#15524 = TOROIDAL_SURFACE ( 'NONE', #8946, 34.90673715956759082, 8.750000000000000000 ) ;
#15525 = DIRECTION ( 'NONE',  ( 0.000000000000000000, 0.000000000000000000, -1.000000000000000000 ) ) ;
#15526 = CARTESIAN_POINT ( 'NONE',  ( -7.325661951454969234, 39.99999999999998579, -52.68655285130741106 ) ) ;
#15527 = DIRECTION ( 'NONE',  ( -1.000000000000000000, 0.000000000000000000, 0.000000000000000000 ) ) ;
#15528 = DIRECTION ( 'NONE',  ( 0.000000000000000000, 0.000000000000000000, 1.000000000000000000 ) ) ;
#15529 = SURFACE_STYLE_USAGE ( .BOTH. , #17489 ) ;
#15530 = EDGE_CURVE ( 'NONE', #22383, #18308, #570, .T. ) ;
#15531 = EDGE_LOOP ( 'NONE', ( #874, #15603, #3167, #16419 ) ) ;
#15532 = CARTESIAN_POINT ( 'NONE',  ( 28.06260833510309993, -14.30873905802335067, 3.000000000000006217 ) ) ;
#15533 = CARTESIAN_POINT ( 'NONE',  ( -16.16773315356748242, 31.81208924699231844, 59.56501305110273137 ) ) ;
#15534 = ORIENTED_EDGE ( 'NONE', *, *, #16095, .F. ) ;
#15535 = DIRECTION ( 'NONE',  ( 6.505213034913038160E-19, 3.903127820947822896E-18, 1.000000000000000000 ) ) ;
#15536 = FACE_OUTER_BOUND ( 'NONE', #1158, .T. ) ;
#15537 = DIRECTION ( 'NONE',  ( -6.505213034913038160E-19, -3.903127820947822896E-18, -1.000000000000000000 ) ) ;
#15538 = CARTESIAN_POINT ( 'NONE',  ( -4.106440533746694932, 34.46303156694462189, 39.55567250430844695 ) ) ;
#15539 = AXIS2_PLACEMENT_3D ( 'NONE', #14519, #5834, #4114 ) ;
#15540 = ORIENTED_EDGE ( 'NONE', *, *, #21889, .T. ) ;
#15541 = AXIS2_PLACEMENT_3D ( 'NONE', #20508, #4815, #11682 ) ;
#15542 = ORIENTED_EDGE ( 'NONE', *, *, #20954, .T. ) ;
#15543 = CIRCLE ( 'NONE', #11888, 41.00000000000000000 ) ;
#15544 = CARTESIAN_POINT ( 'NONE',  ( 6.661198439245855418, -4.819795714534470754, -49.67388352366880611 ) ) ;
#15545 = DIRECTION ( 'NONE',  ( 1.000000000000000000, 0.000000000000000000, 0.000000000000000000 ) ) ;
#15546 = ORIENTED_EDGE ( 'NONE', *, *, #15443, .F. ) ;
#15547 = ADVANCED_FACE ( 'NONE', ( #8869 ), #18883, .T. ) ;
#15548 = CARTESIAN_POINT ( 'NONE',  ( 29.99999999999998579, 20.00000000000000711, 105.0000000000000142 ) ) ;
#15549 = FACE_OUTER_BOUND ( 'NONE', #21542, .T. ) ;
#15550 = DIRECTION ( 'NONE',  ( 0.000000000000000000, 0.000000000000000000, -1.000000000000000000 ) ) ;
#15551 = AXIS2_PLACEMENT_3D ( 'NONE', #2768, #20299, #6309 ) ;
#15552 = CARTESIAN_POINT ( 'NONE',  ( -19.80330599461106544, 22.93419722094641600, -60.57506235960028107 ) ) ;
#15553 = DIRECTION ( 'NONE',  ( 6.505213034913038160E-19, 3.903127820947822896E-18, 1.000000000000000000 ) ) ;
#15554 = EDGE_CURVE ( 'NONE', #7926, #7389, #15991, .T. ) ;
#15555 = CIRCLE ( 'NONE', #22179, 3.399999999999995026 ) ;
#15556 = ORIENTED_EDGE ( 'NONE', *, *, #14354, .F. ) ;
#15557 = CARTESIAN_POINT ( 'NONE',  ( 6.000000000000000888, -40.00000000000000000, 6.000000000000000000 ) ) ;
#15558 = PLANE ( 'NONE',  #21760 ) ;
#15559 = VECTOR ( 'NONE', #18307, 1000.000000000000000 ) ;
#15560 = CARTESIAN_POINT ( 'NONE',  ( 21.99999999999998579, 20.00000000000000000, 98.00000000000000000 ) ) ;
#15561 = DIRECTION ( 'NONE',  ( -1.000000000000000000, -1.208970125616077665E-17, 0.000000000000000000 ) ) ;
#15562 = AXIS2_PLACEMENT_3D ( 'NONE', #2505, #2845, #1122 ) ;
#15563 = ORIENTED_EDGE ( 'NONE', *, *, #12250, .T. ) ;
#15564 = DIRECTION ( 'NONE',  ( -6.505213034913038160E-19, -3.903127820947822896E-18, -1.000000000000000000 ) ) ;
#15565 = DIRECTION ( 'NONE',  ( -0.000000000000000000, 1.000000000000000000, -0.000000000000000000 ) ) ;
#15566 = EDGE_CURVE ( 'NONE', #104, #6092, #6069, .T. ) ;
#15567 = ORIENTED_EDGE ( 'NONE', *, *, #21626, .F. ) ;
#15568 = AXIS2_PLACEMENT_3D ( 'NONE', #17578, #13996, #21025 ) ;
#15569 = AXIS2_PLACEMENT_3D ( 'NONE', #17807, #16078, #19647 ) ;
#15570 = B_SPLINE_CURVE_WITH_KNOTS ( 'NONE', 3,
 ( #18866, #61, #2009, #8543 ),
 .UNSPECIFIED., .F., .F.,
 ( 4, 4 ),
 ( 9.545285770191642639E-07, 0.001900595205834596261 ),
 .UNSPECIFIED. ) ;
#15571 = APPLICATION_PROTOCOL_DEFINITION ( 'draft international standard', 'automotive_design', 1998, #1399 ) ;
#15572 = EDGE_CURVE ( 'NONE', #3415, #9032, #11197, .T. ) ;
#15573 = ORIENTED_EDGE ( 'NONE', *, *, #14020, .F. ) ;
#15574 = CARTESIAN_POINT ( 'NONE',  ( 6.742883674876798850, 34.24928931925766307, 2.999999999999999112 ) ) ;
#15575 = CIRCLE ( 'NONE', #18523, 15.00000000000000000 ) ;
#15576 = CARTESIAN_POINT ( 'NONE',  ( 36.14854559161371128, -0.8615617109689401865, -2.932164912090503339 ) ) ;
#15577 = CARTESIAN_POINT ( 'NONE',  ( -17.66631876130896117, 31.41173278719219653, 3.000000000000016431 ) ) ;
#15578 = CARTESIAN_POINT ( 'NONE',  ( 25.00000000000000000, 20.00000000000000000, 6.487780019669002523E-15 ) ) ;
#15579 = PLANE ( 'NONE',  #2890 ) ;
#15580 = VERTEX_POINT ( 'NONE', #12413 ) ;
#15581 = DIRECTION ( 'NONE',  ( 0.000000000000000000, -1.000000000000000000, 0.000000000000000000 ) ) ;
#15582 = CARTESIAN_POINT ( 'NONE',  ( 35.00000000000000000, 22.00000000000000355, -16.99999999999997868 ) ) ;
#15583 = EDGE_LOOP ( 'NONE', ( #6699, #14836, #11400, #18100 ) ) ;
#15584 = CARTESIAN_POINT ( 'NONE',  ( -0.8499999999999827693, -5.000000000000000000, 48.11213464397150830 ) ) ;
#15585 = CARTESIAN_POINT ( 'NONE',  ( 22.42598460344821376, 19.26775710289564714, -58.66769746720326850 ) ) ;
#15586 = CARTESIAN_POINT ( 'NONE',  ( -35.00000000000000000, 2.142135623730931471, 1.387778780781445676E-14 ) ) ;
#15587 = LINE ( 'NONE', #6906, #19662 ) ;
#15588 = CARTESIAN_POINT ( 'NONE',  ( 13.59841332577228989, 26.34257281673388107, -45.18857684126743379 ) ) ;
#15589 = VERTEX_POINT ( 'NONE', #7269 ) ;
#15590 = DIRECTION ( 'NONE',  ( 0.000000000000000000, 0.000000000000000000, 1.000000000000000000 ) ) ;
#15591 = AXIS2_PLACEMENT_3D ( 'NONE', #13627, #6668, #1513 ) ;
#15592 = AXIS2_PLACEMENT_3D ( 'NONE', #735, #7293, #14139 ) ;
#15593 = CARTESIAN_POINT ( 'NONE',  ( -18.51338123223703747, 7.266791589766472548, 57.69263490290611429 ) ) ;
#15594 = EDGE_LOOP ( 'NONE', ( #20296, #7678, #21453, #21609 ) ) ;
#15595 = DIRECTION ( 'NONE',  ( 6.505213034913038160E-19, 3.903127820947822896E-18, 1.000000000000000000 ) ) ;
#15596 = CARTESIAN_POINT ( 'NONE',  ( -14.30873905802322632, -28.06260833510312835, 2.999999999999995559 ) ) ;
#15597 = CARTESIAN_POINT ( 'NONE',  ( 42.50000000000000711, -12.00000000000012434, 44.97499999999989484 ) ) ;
#15598 = VECTOR ( 'NONE', #8798, 1000.000000000000114 ) ;
#15599 = CARTESIAN_POINT ( 'NONE',  ( 12.91716037299105757, 4.693711897361043661, -55.81219010903327415 ) ) ;
#15600 = EDGE_CURVE ( 'NONE', #8065, #21559, #9732, .T. ) ;
#15601 = ORIENTED_EDGE ( 'NONE', *, *, #13335, .F. ) ;
#15602 = VERTEX_POINT ( 'NONE', #50 ) ;
#15603 = ORIENTED_EDGE ( 'NONE', *, *, #15916, .T. ) ;
#15605 = ADVANCED_FACE ( 'NONE', ( #17684 ), #14481, .F. ) ;
#15604 =( LENGTH_UNIT ( ) NAMED_UNIT ( * ) SI_UNIT ( .MILLI., .METRE. ) );
#15606 = EDGE_CURVE ( 'NONE', #18457, #3259, #21353, .T. ) ;
#15607 = VECTOR ( 'NONE', #1369, 1000.000000000000000 ) ;
#15608 = VERTEX_POINT ( 'NONE', #5653 ) ;
#15609 = DIRECTION ( 'NONE',  ( 0.000000000000000000, -0.000000000000000000, 1.000000000000000000 ) ) ;
#15610 = CARTESIAN_POINT ( 'NONE',  ( 13.67681338760603715, 37.77871559274756663, 56.08437820317178080 ) ) ;
#15611 = CARTESIAN_POINT ( 'NONE',  ( 8.845644329309713783, 39.99999999999999289, -53.28398128908064280 ) ) ;
#15612 = CARTESIAN_POINT ( 'NONE',  ( 1.387778780781445676E-14, 40.00000000000000000, 48.73397172404482802 ) ) ;
#15613 = EDGE_LOOP ( 'NONE', ( #20549, #16881, #18320, #7782 ) ) ;
#15614 = CARTESIAN_POINT ( 'NONE',  ( 0.000000000000000000, 30.00000000000000000, 3.999999999999996447 ) ) ;
#15615 = DIRECTION ( 'NONE',  ( 0.000000000000000000, 0.000000000000000000, 1.000000000000000000 ) ) ;
#15616 = VERTEX_POINT ( 'NONE', #13997 ) ;
#15617 = ORIENTED_EDGE ( 'NONE', *, *, #16314, .F. ) ;
#15618 = CARTESIAN_POINT ( 'NONE',  ( -2.999999999999999112, 30.00000000000000000, 8.485281374238567764 ) ) ;
#15619 = ORIENTED_EDGE ( 'NONE', *, *, #18211, .T. ) ;
#15620 = CARTESIAN_POINT ( 'NONE',  ( 6.297084008441820480, 38.99689388921666477, -53.73982653936155174 ) ) ;
#15621 = EDGE_CURVE ( 'NONE', #10947, #1869, #15838, .T. ) ;
#15622 = CARTESIAN_POINT ( 'NONE',  ( -16.99647590252643781, -30.48934413892778750, -2.999999999999992450 ) ) ;
#15623 = CARTESIAN_POINT ( 'NONE',  ( -2.232801763152736818, 39.96997183162479672, 50.39091575928458155 ) ) ;
#15624 = VECTOR ( 'NONE', #8056, 1000.000000000000000 ) ;
#15625 = CARTESIAN_POINT ( 'NONE',  ( 17.42297160866501571, 10.14068842408646809, 59.94615209474302020 ) ) ;
#15626 = CARTESIAN_POINT ( 'NONE',  ( 25.58633464742632313, 23.74488952252767859, -2.999999999999971578 ) ) ;
#15627 = CIRCLE ( 'NONE', #3580, 18.00000000000000000 ) ;
#15628 = DIRECTION ( 'NONE',  ( 0.000000000000000000, 0.000000000000000000, 1.000000000000000000 ) ) ;
#15629 = VERTEX_POINT ( 'NONE', #21026 ) ;
#15630 = VERTEX_POINT ( 'NONE', #3835 ) ;
#15631 = AXIS2_PLACEMENT_3D ( 'NONE', #6679, #22618, #20654 ) ;
#15632 = VECTOR ( 'NONE', #7475, 1000.000000000000000 ) ;
#15633 = ORIENTED_EDGE ( 'NONE', *, *, #17163, .T. ) ;
#15634 = ORIENTED_EDGE ( 'NONE', *, *, #5213, .F. ) ;
#15635 = DIRECTION ( 'NONE',  ( 6.505213034913038160E-19, 3.903127820947822896E-18, 1.000000000000000000 ) ) ;
#15636 = DIRECTION ( 'NONE',  ( 1.000000000000000000, 0.000000000000000000, 0.000000000000000000 ) ) ;
#15637 = AXIS2_PLACEMENT_3D ( 'NONE', #21810, #22377, #20877 ) ;
#15638 = B_SPLINE_CURVE_WITH_KNOTS ( 'NONE', 1,
 ( #10419, #8383 ),
 .UNSPECIFIED., .F., .F.,
 ( 2, 2 ),
 ( 0.000000000000000000, 1.000000000000000000 ),
 .UNSPECIFIED. ) ;
#15639 = CIRCLE ( 'NONE', #1370, 31.50000000000000711 ) ;
#15640 = CARTESIAN_POINT ( 'NONE',  ( -11.49398617736659034, 40.00000000000000711, -54.13866599136176205 ) ) ;
#15641 = DIRECTION ( 'NONE',  ( -1.000000000000000000, 0.000000000000000000, 0.000000000000000000 ) ) ;
#15642 = CARTESIAN_POINT ( 'NONE',  ( 6.571663212755819217, 39.72078165691683438, 53.11617168483076057 ) ) ;
#15643 = AXIS2_PLACEMENT_3D ( 'NONE', #21980, #19906, #12672 ) ;
#15644 = ADVANCED_FACE ( 'NONE', ( #10799 ), #10464, .T. ) ;
#15645 = ADVANCED_FACE ( 'NONE', ( #3951 ), #10580, .T. ) ;
#15646 = ORIENTED_EDGE ( 'NONE', *, *, #12524, .F. ) ;
#15647 = CARTESIAN_POINT ( 'NONE',  ( 30.07487443287978834, -12.31876324338301920, 3.000000000000023537 ) ) ;
#15648 = CARTESIAN_POINT ( 'NONE',  ( -7.158017810174624351, 39.99999999999999289, -52.61520711206481593 ) ) ;
#15649 = DIRECTION ( 'NONE',  ( 0.000000000000000000, 0.000000000000000000, -1.000000000000000000 ) ) ;
#15650 = DIRECTION ( 'NONE',  ( 1.208970125616062874E-17, -1.000000000000000000, 3.903127820947822896E-18 ) ) ;
#15651 = CARTESIAN_POINT ( 'NONE',  ( 27.64365646977287483, 17.09029715894919121, -2.999999999999975131 ) ) ;
#15652 = ORIENTED_EDGE ( 'NONE', *, *, #5687, .T. ) ;
#15653 = VECTOR ( 'NONE', #10470, 1000.000000000000000 ) ;
#15654 = ADVANCED_FACE ( 'NONE', ( #21135 ), #18164, .T. ) ;
#15655 = AXIS2_PLACEMENT_3D ( 'NONE', #19187, #41, #13657 ) ;
#15656 = AXIS2_PLACEMENT_3D ( 'NONE', #10755, #21661, #5505 ) ;
#15657 = PLANE ( 'NONE',  #1967 ) ;
#15658 = PLANE ( 'NONE',  #13331 ) ;
#15659 = CIRCLE ( 'NONE', #9816, 3.999999999999998224 ) ;
#15660 = DIRECTION ( 'NONE',  ( 0.000000000000000000, -1.000000000000000000, 0.000000000000000000 ) ) ;
#15661 = CIRCLE ( 'NONE', #16775, 0.9999999999999991118 ) ;
#15662 = VERTEX_POINT ( 'NONE', #2223 ) ;
#15663 = ORIENTED_EDGE ( 'NONE', *, *, #20748, .F. ) ;
#15664 = VERTEX_POINT ( 'NONE', #9661 ) ;
#15665 = CARTESIAN_POINT ( 'NONE',  ( -6.742883674876437361, -34.24928931925796860, 3.000000000000002665 ) ) ;
#15666 = VECTOR ( 'NONE', #17142, 1000.000000000000114 ) ;
#15667 = CARTESIAN_POINT ( 'NONE',  ( 11.28246622563954915, 40.00000000000000000, -54.06713842414182380 ) ) ;
#15668 = ORIENTED_EDGE ( 'NONE', *, *, #15091, .F. ) ;
#15669 = CIRCLE ( 'NONE', #16786, 12.00000000000000000 ) ;
#15670 = AXIS2_PLACEMENT_3D ( 'NONE', #2383, #10730, #9374 ) ;
#15671 = PLANE ( 'NONE',  #21618 ) ;
#15672 = LINE ( 'NONE', #15434, #11790 ) ;
#15673 = CYLINDRICAL_SURFACE ( 'NONE', #8698, 16.49999999999999645 ) ;
#15674 = CARTESIAN_POINT ( 'NONE',  ( -20.00295458799181247, 20.28336436466281612, -60.62247787804551535 ) ) ;
#15675 = AXIS2_PLACEMENT_3D ( 'NONE', #18096, #2411, #3372 ) ;
#15676 = CARTESIAN_POINT ( 'NONE',  ( 35.00000000000000000, 2.142135623730931471, 4.258610482196280173E-15 ) ) ;
#15677 = B_SPLINE_SURFACE_WITH_KNOTS ( 'NONE', 3, 1, ( 
 ( #2704, #6591 ),
 ( #20347, #13553 ),
 ( #4872, #16898 ),
 ( #11401, #18631 ),
 ( #4538, #17002 ),
 ( #11519, #21519 ),
 ( #2816, #542 ),
 ( #6139, #4425 ),
 ( #9800, #9246 ),
 ( #13107, #2935 ) ),
 .UNSPECIFIED., .F., .F., .F.,
 ( 4, 2, 2, 2, 4 ),
 ( 2, 2 ),
 ( 0.000000000000000000, 0.2500000000000000000, 0.5000000000000000000, 0.7500000000000000000, 1.000000000000000000 ),
 ( 0.000000000000000000, 1.000000000000000000 ),
 .UNSPECIFIED. ) ;
#15678 = ORIENTED_EDGE ( 'NONE', *, *, #21210, .T. ) ;
#15679 = CARTESIAN_POINT ( 'NONE',  ( 7.325260514639500961E-15, -4.648749848371387827, 45.43309249825157536 ) ) ;
#15680 = CARTESIAN_POINT ( 'NONE',  ( 15.49999999999993783, 42.51666049839543149, 60.00099999999999767 ) ) ;
#15681 = CARTESIAN_POINT ( 'NONE',  ( -9.576564013118820995, 26.31139338200511091, 2.999999999999999112 ) ) ;
#15682 = CARTESIAN_POINT ( 'NONE',  ( -35.00000000000000000, -4.999999999999997335, 1.387778780781445676E-14 ) ) ;
#15683 = EDGE_LOOP ( 'NONE', ( #16588, #19045 ) ) ;
#15684 = COLOUR_RGB ( '',0.7921568627450980005, 0.8196078431372548767, 0.9333333333333333481 ) ;
#15685 = DIRECTION ( 'NONE',  ( 6.505213034913038160E-19, 3.903127820947822896E-18, 1.000000000000000000 ) ) ;
#15686 = CARTESIAN_POINT ( 'NONE',  ( 35.00000000000000000, 40.00000000000000000, 4.258610482196280173E-15 ) ) ;
#15687 = VECTOR ( 'NONE', #3689, 1000.000000000000000 ) ;
#15688 = EDGE_CURVE ( 'NONE', #7803, #17903, #5999, .T. ) ;
#15689 = PRODUCT_DEFINITION_FORMATION_WITH_SPECIFIED_SOURCE ( 'ANY', '', #10941, .NOT_KNOWN. ) ;
#15690 = ORIENTED_EDGE ( 'NONE', *, *, #14720, .T. ) ;
#15691 = EDGE_CURVE ( 'NONE', #9986, #2332, #3143, .T. ) ;
#15692 = CONTEXT_DEPENDENT_SHAPE_REPRESENTATION ( #2883, #16624 ) ;
#15693 = ORIENTED_EDGE ( 'NONE', *, *, #12082, .F. ) ;
#15694 = CARTESIAN_POINT ( 'NONE',  ( 89.99999999999701572, -5.000000000000000000, 2.499999999999956479 ) ) ;
#15695 = CARTESIAN_POINT ( 'NONE',  ( 9.103081159019511759, 0.03030367950604065386, -53.87333532811885561 ) ) ;
#15696 = DIRECTION ( 'NONE',  ( 0.000000000000000000, 0.000000000000000000, -1.000000000000000000 ) ) ;
#15697 = DIRECTION ( 'NONE',  ( -0.000000000000000000, -0.000000000000000000, -1.000000000000000000 ) ) ;
#15698 = ORIENTED_EDGE ( 'NONE', *, *, #594, .F. ) ;
#15699 = CARTESIAN_POINT ( 'NONE',  ( 0.000000000000000000, -45.00000000000000000, 0.000000000000000000 ) ) ;
#15700 = CARTESIAN_POINT ( 'NONE',  ( -10.95224849132202927, 40.00000000000000711, -53.95427542910578467 ) ) ;
#15701 = EDGE_LOOP ( 'NONE', ( #898, #11183, #6221, #16977, #17577, #12204 ) ) ;
#15702 = CARTESIAN_POINT ( 'NONE',  ( -18.00000000000001421, 20.00000000000000355, -102.0000000000000142 ) ) ;
#15703 = CARTESIAN_POINT ( 'NONE',  ( 18.35281960068861196, 33.06122318964057172, -57.65236019522514965 ) ) ;
#15704 = CARTESIAN_POINT ( 'NONE',  ( -35.00000000000000000, 0.000000000000000000, -8.999999999999989342 ) ) ;
#15705 = CARTESIAN_POINT ( 'NONE',  ( 1.485224240694672737, 39.99052334830943778, 49.86416386702911296 ) ) ;
#15706 = CARTESIAN_POINT ( 'NONE',  ( -1.387778780781474075E-14, 40.00000000000002132, -48.73397172404482092 ) ) ;
#15707 = ADVANCED_FACE ( 'NONE', ( #4173 ), #21472, .F. ) ;
#15708 = ORIENTED_EDGE ( 'NONE', *, *, #22073, .F. ) ;
#15709 = CARTESIAN_POINT ( 'NONE',  ( 2.602085213965210642E-15, 6.000000000000019540, 17.00000000000000355 ) ) ;
#15710 = DIRECTION ( 'NONE',  ( 6.505213034913038160E-19, 3.903127820947822896E-18, 1.000000000000000000 ) ) ;
#15711 = ORIENTED_EDGE ( 'NONE', *, *, #1342, .T. ) ;
#15712 = CARTESIAN_POINT ( 'NONE',  ( -3.999999999999996447, -1.500000000000014877, 0.000000000000000000 ) ) ;
#15713 = CARTESIAN_POINT ( 'NONE',  ( 42.50000000000000711, -5.000000000000000000, -47.50000000000000000 ) ) ;
#15714 = ADVANCED_FACE ( 'NONE', ( #11496 ), #14111, .T. ) ;
#15715 = CIRCLE ( 'NONE', #21596, 36.76383501243555685 ) ;
#15716 = ORIENTED_EDGE ( 'NONE', *, *, #6147, .T. ) ;
#15717 = EDGE_CURVE ( 'NONE', #8015, #15814, #21447, .T. ) ;
#15718 = ORIENTED_EDGE ( 'NONE', *, *, #6645, .T. ) ;
#15719 = ORIENTED_EDGE ( 'NONE', *, *, #22469, .T. ) ;
#15720 = VERTEX_POINT ( 'NONE', #16850 ) ;
#15721 = CARTESIAN_POINT ( 'NONE',  ( 1.665334536937734811E-13, 2.999999999999780620, 5.000000000000022204 ) ) ;
#15722 = CARTESIAN_POINT ( 'NONE',  ( 20.67483659015367436, 11.23071942442634885, 58.26617649125748954 ) ) ;
#15723 = AXIS2_PLACEMENT_3D ( 'NONE', #11341, #21656, #15090 ) ;
#15724 = CARTESIAN_POINT ( 'NONE',  ( 0.000000000000000000, 0.000000000000000000, 0.000000000000000000 ) ) ;
#15725 = CARTESIAN_POINT ( 'NONE',  ( 9.233659691198207398, 40.00000000000000000, 53.41795191989319136 ) ) ;
#15726 = SHAPE_REPRESENTATION ( 'REAR COVER', ( #18273 ), #22313 ) ;
#15727 = VERTEX_POINT ( 'NONE', #9958 ) ;
#15728 = DIRECTION ( 'NONE',  ( 0.000000000000000000, -1.000000000000000000, 0.000000000000000000 ) ) ;
#15729 = CYLINDRICAL_SURFACE ( 'NONE', #6623, 31.50000000000000711 ) ;
#15730 = ORIENTED_EDGE ( 'NONE', *, *, #11936, .F. ) ;
#15731 = DIRECTION ( 'NONE',  ( 0.000000000000000000, 0.000000000000000000, 1.000000000000000000 ) ) ;
#15732 = DIRECTION ( 'NONE',  ( -0.000000000000000000, 1.000000000000000000, -0.000000000000000000 ) ) ;
#15733 = VERTEX_POINT ( 'NONE', #4820 ) ;
#15734 = EDGE_CURVE ( 'NONE', #22134, #2949, #1489, .T. ) ;
#15735 = DIRECTION ( 'NONE',  ( 0.000000000000000000, 0.000000000000000000, -1.000000000000000000 ) ) ;
#15736 = VERTEX_POINT ( 'NONE', #4481 ) ;
#15737 = CARTESIAN_POINT ( 'NONE',  ( 2.881564033229496502, 39.80724459714780750, -51.34429167881276612 ) ) ;
#15738 = CARTESIAN_POINT ( 'NONE',  ( -22.12933039895920828, 28.19616000222404040, 0.000000000000000000 ) ) ;
#15739 = CARTESIAN_POINT ( 'NONE',  ( 89.99999999999701572, -5.000000000000000000, -5.216535399428728743E-14 ) ) ;
#15740 = CARTESIAN_POINT ( 'NONE',  ( 20.00295458799178405, 20.28336436466281612, 60.62247787804552956 ) ) ;
#15741 = DIRECTION ( 'NONE',  ( 0.000000000000000000, 1.000000000000000000, 0.000000000000000000 ) ) ;
#15742 = EDGE_CURVE ( 'NONE', #13563, #18413, #12646, .T. ) ;
#15743 = ADVANCED_FACE ( 'NONE', ( #22241 ), #8033, .F. ) ;
#15744 = AXIS2_PLACEMENT_3D ( 'NONE', #22577, #20852, #1361 ) ;
#15745 = CYLINDRICAL_SURFACE ( 'NONE', #8204, 19.11328065563151668 ) ;
#15746 = EDGE_LOOP ( 'NONE', ( #12738, #9698 ) ) ;
#15747 = VERTEX_POINT ( 'NONE', #1256 ) ;
#15748 = VERTEX_POINT ( 'NONE', #18791 ) ;
#15749 = ORIENTED_EDGE ( 'NONE', *, *, #10885, .F. ) ;
#15750 = CARTESIAN_POINT ( 'NONE',  ( -1.387778780781445676E-14, 20.00000000000000000, 102.0000000000000142 ) ) ;
#15751 = DIRECTION ( 'NONE',  ( 6.505213034913038160E-19, 3.903127820947822896E-18, 1.000000000000000000 ) ) ;
#15752 = EDGE_CURVE ( 'NONE', #16159, #3040, #18518, .T. ) ;
#15753 = AXIS2_PLACEMENT_3D ( 'NONE', #14366, #4313, #10821 ) ;
#15754 = CARTESIAN_POINT ( 'NONE',  ( -42.50000000000000711, -12.00000000000000000, -54.00000000000000000 ) ) ;
#15755 = CARTESIAN_POINT ( 'NONE',  ( 0.02448413884701040183, 39.99999651920320076, 48.75302353242081210 ) ) ;
#15756 = B_SPLINE_CURVE_WITH_KNOTS ( 'NONE', 3,
 ( #19764, #3727, #4070, #3952 ),
 .UNSPECIFIED., .F., .F.,
 ( 4, 4 ),
 ( 9.545285771901622165E-07, 0.001900595205834791634 ),
 .UNSPECIFIED. ) ;
#15757 = CIRCLE ( 'NONE', #16113, 58.99999999999994316 ) ;
#15758 = EDGE_CURVE ( 'NONE', #9978, #20188, #3095, .T. ) ;
#15759 = ORIENTED_EDGE ( 'NONE', *, *, #10401, .T. ) ;
#15760 = DIRECTION ( 'NONE',  ( 0.000000000000000000, 0.000000000000000000, 1.000000000000000000 ) ) ;
#15761 = DIRECTION ( 'NONE',  ( -0.000000000000000000, 1.000000000000000000, -0.000000000000000000 ) ) ;
#15762 = LINE ( 'NONE', #70, #22280 ) ;
#15763 = LINE ( 'NONE', #19674, #6060 ) ;
#15764 =( NAMED_UNIT ( * ) SI_UNIT ( $, .STERADIAN. ) SOLID_ANGLE_UNIT ( ) );
#15765 = CIRCLE ( 'NONE', #19088, 2.525000000000110489 ) ;
#15766 = CARTESIAN_POINT ( 'NONE',  ( -9.786577258570266835, 39.51695195164889896, 54.52237260331529001 ) ) ;
#15767 = FACE_OUTER_BOUND ( 'NONE', #12097, .T. ) ;
#15768 = DIRECTION ( 'NONE',  ( -1.000000000000000000, 0.000000000000000000, 0.000000000000000000 ) ) ;
#15769 = EDGE_CURVE ( 'NONE', #9340, #3496, #13016, .T. ) ;
#15770 = ORIENTED_EDGE ( 'NONE', *, *, #12330, .T. ) ;
#15771 = ORIENTED_EDGE ( 'NONE', *, *, #5547, .F. ) ;
#15772 = EDGE_LOOP ( 'NONE', ( #12431, #13495, #15534, #18940 ) ) ;
#15773 = CARTESIAN_POINT ( 'NONE',  ( -36.06598984771569860, 10.00000000000000000, -48.42385786802031333 ) ) ;
#15774 = DIRECTION ( 'NONE',  ( -6.505213034913038160E-19, -3.903127820947822896E-18, -1.000000000000000000 ) ) ;
#15775 = ORIENTED_EDGE ( 'NONE', *, *, #19535, .T. ) ;
#15776 = AXIS2_PLACEMENT_3D ( 'NONE', #14099, #9310, #7587 ) ;
#15777 = DIRECTION ( 'NONE',  ( -0.000000000000000000, 1.000000000000000000, -0.000000000000000000 ) ) ;
#15778 = CARTESIAN_POINT ( 'NONE',  ( 16.66666666666666430, 20.00000000000000000, 23.57022603955159212 ) ) ;
#15779 = CARTESIAN_POINT ( 'NONE',  ( -35.99819890246953946, 7.463862311151231665, 2.800654218530509443 ) ) ;
#15780 = CARTESIAN_POINT ( 'NONE',  ( -16.16619463698821946, 31.79081685853821782, -57.00191113791401420 ) ) ;
#15781 = LINE ( 'NONE', #202, #17022 ) ;
#15782 = ORIENTED_EDGE ( 'NONE', *, *, #13219, .F. ) ;
#15783 = CARTESIAN_POINT ( 'NONE',  ( 9.103081159019511759, 0.03030367950604059835, -53.87333532811884851 ) ) ;
#15784 = FACE_OUTER_BOUND ( 'NONE', #10288, .T. ) ;
#15785 = FACE_OUTER_BOUND ( 'NONE', #20364, .T. ) ;
#15786 = CARTESIAN_POINT ( 'NONE',  ( 13.25963002225075194, 12.97669314386527439, -45.02656532858657101 ) ) ;
#15787 = VERTEX_POINT ( 'NONE', #6760 ) ;
#15788 = DIRECTION ( 'NONE',  ( -6.505213034913038160E-19, -3.903127820947822896E-18, -1.000000000000000000 ) ) ;
#15789 = CARTESIAN_POINT ( 'NONE',  ( 3.330669073875469621E-13, -1.110223024625156540E-13, -2.999999999999971578 ) ) ;
#15790 = EDGE_CURVE ( 'NONE', #5071, #15629, #19619, .T. ) ;
#15791 = CIRCLE ( 'NONE', #14331, 2.099999999999990763 ) ;
#15792 = EDGE_LOOP ( 'NONE', ( #7168, #14371, #15821, #13656 ) ) ;
#15793 = ADVANCED_FACE ( 'NONE', ( #15337 ), #339, .F. ) ;
#15794 = ORIENTED_EDGE ( 'NONE', *, *, #7647, .F. ) ;
#15795 = FACE_OUTER_BOUND ( 'NONE', #11389, .T. ) ;
#15796 = CARTESIAN_POINT ( 'NONE',  ( 1.522021317816235619, -4.618502324873039022, 46.61386490714507147 ) ) ;
#15797 = CARTESIAN_POINT ( 'NONE',  ( 13.85640646055130709, -25.00000000000000000, -8.000000000000097700 ) ) ;
#15798 = DIRECTION ( 'NONE',  ( -1.000000000000000000, -1.208970125616060101E-17, 6.505213034913038160E-19 ) ) ;
#15799 = CARTESIAN_POINT ( 'NONE',  ( 35.00000000000000711, 2.142135623730931471, 60.00000000000000711 ) ) ;
#15800 = VERTEX_POINT ( 'NONE', #18684 ) ;
#15801 = CARTESIAN_POINT ( 'NONE',  ( 12.31876324338274031, 30.07487443287973505, -2.999999999999999112 ) ) ;
#15802 = DIRECTION ( 'NONE',  ( -0.000000000000000000, 1.000000000000000000, -0.000000000000000000 ) ) ;
#15803 = ORIENTED_EDGE ( 'NONE', *, *, #10117, .F. ) ;
#15804 = DIRECTION ( 'NONE',  ( -6.505213034913038160E-19, -3.903127820947822896E-18, -1.000000000000000000 ) ) ;
#15805 = EDGE_CURVE ( 'NONE', #19486, #4351, #6833, .T. ) ;
#15806 = DIRECTION ( 'NONE',  ( -0.000000000000000000, -1.000000000000000000, -0.000000000000000000 ) ) ;
#15807 = AXIS2_PLACEMENT_3D ( 'NONE', #14046, #2159, #16233 ) ;
#15808 = CIRCLE ( 'NONE', #18754, 57.00000000000002132 ) ;
#15809 = DIRECTION ( 'NONE',  ( -1.000000000000000000, 0.000000000000000000, 0.000000000000000000 ) ) ;
#15810 = CARTESIAN_POINT ( 'NONE',  ( -8.776846322808903977, 39.47243301020848349, -54.19537465121766928 ) ) ;
#15811 = VERTEX_POINT ( 'NONE', #9861 ) ;
#15812 = DIRECTION ( 'NONE',  ( 1.000000000000000000, 1.208970125616186904E-17, 0.000000000000000000 ) ) ;
#15813 = CARTESIAN_POINT ( 'NONE',  ( -3.655629734721801416, 39.91824796244861773, -51.36063886735895068 ) ) ;
#15814 = VERTEX_POINT ( 'NONE', #6643 ) ;
#15815 = EDGE_CURVE ( 'NONE', #57, #8887, #16685, .T. ) ;
#15816 = DIRECTION ( 'NONE',  ( -0.1421319796954317316, 0.000000000000000000, 0.9898477157360405787 ) ) ;
#15817 = FACE_OUTER_BOUND ( 'NONE', #7963, .T. ) ;
#15818 = ORIENTED_EDGE ( 'NONE', *, *, #1866, .T. ) ;
#15819 = CIRCLE ( 'NONE', #8885, 19.00000000000000355 ) ;
#15820 = VERTEX_POINT ( 'NONE', #20406 ) ;
#15821 = ORIENTED_EDGE ( 'NONE', *, *, #2716, .T. ) ;
#15822 = AXIS2_PLACEMENT_3D ( 'NONE', #10806, #21478, #12757 ) ;
#15823 = VERTEX_POINT ( 'NONE', #17177 ) ;
#15824 = DIRECTION ( 'NONE',  ( -0.000000000000000000, 1.000000000000000000, -0.000000000000000000 ) ) ;
#15825 = DIRECTION ( 'NONE',  ( 0.000000000000000000, 0.000000000000000000, -1.000000000000000000 ) ) ;
#15826 = DIRECTION ( 'NONE',  ( -1.000000000000000000, -1.208970125616060717E-17, 0.000000000000000000 ) ) ;
#15827 = CARTESIAN_POINT ( 'NONE',  ( 2.783900019938605919, 39.99999999999999289, 50.42898711214131424 ) ) ;
#15828 = VERTEX_POINT ( 'NONE', #4715 ) ;
#15829 = FACE_BOUND ( 'NONE', #2929, .T. ) ;
#15830 = DIRECTION ( 'NONE',  ( 0.000000000000000000, -1.000000000000000000, 0.000000000000000000 ) ) ;
#15831 = VERTEX_POINT ( 'NONE', #10518 ) ;
#15832 = ADVANCED_FACE ( 'NONE', ( #1834 ), #17522, .F. ) ;
#15833 = CARTESIAN_POINT ( 'NONE',  ( -16.62266455332489201, 35.11598757108757241, -57.12012504743137953 ) ) ;
#15834 = DIRECTION ( 'NONE',  ( -1.000000000000000000, 0.000000000000000000, 0.000000000000000000 ) ) ;
#15835 = ORIENTED_EDGE ( 'NONE', *, *, #10402, .T. ) ;
#15836 = DIRECTION ( 'NONE',  ( 6.505213034913038160E-19, 3.903127820947822896E-18, 1.000000000000000000 ) ) ;
#15837 = EDGE_LOOP ( 'NONE', ( #5250, #4862 ) ) ;
#15838 = LINE ( 'NONE', #19527, #2798 ) ;
#15839 = CARTESIAN_POINT ( 'NONE',  ( -2.669020651088310103, 39.95797167561620711, 50.69824585152028362 ) ) ;
#15840 = ADVANCED_FACE ( 'NONE', ( #5271 ), #15896, .F. ) ;
#15841 = CIRCLE ( 'NONE', #18402, 27.99999999999999645 ) ;
#15842 = CARTESIAN_POINT ( 'NONE',  ( 19.39432138270210260, 15.03492235294207546, 60.47577240662250375 ) ) ;
#15843 = DIRECTION ( 'NONE',  ( 8.659560562351929024E-17, -0.7071067811867928210, 0.7071067811863022134 ) ) ;
#15844 = CIRCLE ( 'NONE', #3793, 2.099999999999997868 ) ;
#15845 = CIRCLE ( 'NONE', #12546, 10.00000000000000000 ) ;
#15846 = CARTESIAN_POINT ( 'NONE',  ( 10.49999999999994316, 42.51666049839543149, -100.0000000000000000 ) ) ;
#15847 = VERTEX_POINT ( 'NONE', #17282 ) ;
#15848 = AXIS2_PLACEMENT_3D ( 'NONE', #2601, #11178, #2370 ) ;
#15849 = VERTEX_POINT ( 'NONE', #16017 ) ;
#15850 = ADVANCED_FACE ( 'NONE', ( #5050, #19471, #12030, #19369, #1597, #8585, #3336, #15785 ), #6877, .T. ) ;
#15851 = AXIS2_PLACEMENT_3D ( 'NONE', #5675, #7739, #859 ) ;
#15852 = ORIENTED_EDGE ( 'NONE', *, *, #9867, .F. ) ;
#15853 = VERTEX_POINT ( 'NONE', #13722 ) ;
#15854 = DIRECTION ( 'NONE',  ( -6.505213034913038160E-19, -3.903127820947822896E-18, -1.000000000000000000 ) ) ;
#15855 = DIRECTION ( 'NONE',  ( 0.000000000000000000, 1.000000000000000000, 0.000000000000000000 ) ) ;
#15856 = VECTOR ( 'NONE', #897, 1000.000000000000000 ) ;
#15857 = DIRECTION ( 'NONE',  ( -6.505213034913038160E-19, -3.903127820947822896E-18, -1.000000000000000000 ) ) ;
#15858 = CARTESIAN_POINT ( 'NONE',  ( 0.1974762773663032156, 39.99977543037353911, 48.88709678338103259 ) ) ;
#15859 = EDGE_CURVE ( 'NONE', #18194, #17863, #22193, .T. ) ;
#15860 = EDGE_CURVE ( 'NONE', #13273, #8612, #10834, .T. ) ;
#15861 = AXIS2_PLACEMENT_3D ( 'NONE', #5055, #6764, #17528 ) ;
#15862 = ORIENTED_EDGE ( 'NONE', *, *, #6122, .T. ) ;
#15863 = CARTESIAN_POINT ( 'NONE',  ( 2.347663744114520057, 31.41239365194192601, -6.999999999999950262 ) ) ;
#15864 = DIRECTION ( 'NONE',  ( -0.000000000000000000, -0.000000000000000000, 1.000000000000000000 ) ) ;
#15865 = DIRECTION ( 'NONE',  ( 0.000000000000000000, 0.000000000000000000, 1.000000000000000000 ) ) ;
#15866 = LINE ( 'NONE', #9230, #8250 ) ;
#15867 =( NAMED_UNIT ( * ) SI_UNIT ( $, .STERADIAN. ) SOLID_ANGLE_UNIT ( ) );
#15868 = AXIS2_PLACEMENT_3D ( 'NONE', #18360, #15250, #13529 ) ;
#15869 = DIRECTION ( 'NONE',  ( -0.000000000000000000, -1.000000000000000000, -0.000000000000000000 ) ) ;
#15870 = AXIS2_PLACEMENT_3D ( 'NONE', #16003, #5152, #3660 ) ;
#15871 = FACE_BOUND ( 'NONE', #5020, .T. ) ;
#15872 = CARTESIAN_POINT ( 'NONE',  ( 22.15900668633799597, 29.33526866242094755, 2.800654218530481465 ) ) ;
#15873 = CARTESIAN_POINT ( 'NONE',  ( -24.73600648735115115, 27.19760187735867518, 2.800654218530485018 ) ) ;
#15874 =( GEOMETRIC_REPRESENTATION_CONTEXT ( 3 ) GLOBAL_UNCERTAINTY_ASSIGNED_CONTEXT ( ( #7806 ) ) GLOBAL_UNIT_ASSIGNED_CONTEXT ( ( #12569, #17627, #10735 ) ) REPRESENTATION_CONTEXT ( 'NONE', 'WORKASPACE' ) );
#15875 = VERTEX_POINT ( 'NONE', #17400 ) ;
#15876 = EDGE_LOOP ( 'NONE', ( #19578, #8125, #12929, #10341 ) ) ;
#15877 = EDGE_CURVE ( 'NONE', #7803, #2693, #3442, .T. ) ;
#15878 = ORIENTED_EDGE ( 'NONE', *, *, #22211, .F. ) ;
#15879 = CARTESIAN_POINT ( 'NONE',  ( 9.327259721472362486, -2.742977016014242597, -53.40697688051515968 ) ) ;
#15880 = AXIS2_PLACEMENT_3D ( 'NONE', #6568, #22153, #6450 ) ;
#15881 = CARTESIAN_POINT ( 'NONE',  ( 9.952189117650862116, 40.00000000000000000, -53.64426396172072486 ) ) ;
#15882 = EDGE_CURVE ( 'NONE', #11599, #13122, #9382, .T. ) ;
#15883 = EDGE_CURVE ( 'NONE', #6097, #7816, #3536, .T. ) ;
#15884 = EDGE_CURVE ( 'NONE', #20081, #4381, #8919, .T. ) ;
#15885 = VECTOR ( 'NONE', #22103, 1000.000000000000000 ) ;
#15886 = DIRECTION ( 'NONE',  ( 1.000000000000000000, 1.208970125616063028E-17, 0.000000000000000000 ) ) ;
#15887 = CARTESIAN_POINT ( 'NONE',  ( 35.00000000000000711, -4.928932188134504955, -57.07106781186551103 ) ) ;
#15888 = CARTESIAN_POINT ( 'NONE',  ( -33.51030287062373247, -15.12081897056669000, -2.800654218530457484 ) ) ;
#15889 = CARTESIAN_POINT ( 'NONE',  ( 5.999999999999999112, -40.00000000000000000, -6.000000000000000000 ) ) ;
#15890 = FACE_OUTER_BOUND ( 'NONE', #3325, .T. ) ;
#15891 = VERTEX_POINT ( 'NONE', #20859 ) ;
#15892 = DIRECTION ( 'NONE',  ( 0.000000000000000000, 0.000000000000000000, 1.000000000000000000 ) ) ;
#15893 = PLANE ( 'NONE',  #16209 ) ;
#15894 = EDGE_CURVE ( 'NONE', #5664, #22110, #21076, .T. ) ;
#15895 =( NAMED_UNIT ( * ) SI_UNIT ( $, .STERADIAN. ) SOLID_ANGLE_UNIT ( ) );
#15896 = CYLINDRICAL_SURFACE ( 'NONE', #10459, 3.999999999999998224 ) ;
#15897 = AXIS2_PLACEMENT_3D ( 'NONE', #2851, #2965, #1666 ) ;
#15898 = CARTESIAN_POINT ( 'NONE',  ( -26.00000000000001421, 19.99999999999982947, -100.0000000000000000 ) ) ;
#15899 = ORIENTED_EDGE ( 'NONE', *, *, #4622, .F. ) ;
#15900 = DIRECTION ( 'NONE',  ( 1.000000000000000000, 0.000000000000000000, 0.000000000000000000 ) ) ;
#15901 = DIRECTION ( 'NONE',  ( -1.000000000000000000, -1.208970125616081209E-17, 0.000000000000000000 ) ) ;
#15902 = CIRCLE ( 'NONE', #21802, 51.00000000000001421 ) ;
#15903 = VERTEX_POINT ( 'NONE', #12357 ) ;
#15904 = CIRCLE ( 'NONE', #12280, 18.00000000000000000 ) ;
#15905 = ORIENTED_EDGE ( 'NONE', *, *, #12811, .F. ) ;
#15906 = CARTESIAN_POINT ( 'NONE',  ( -2.999999999999998668, 22.79887287893604153, 6.485281374238567764 ) ) ;
#15907 = VECTOR ( 'NONE', #15095, 1000.000000000000000 ) ;
#15908 = DIRECTION ( 'NONE',  ( 1.000000000000000000, 0.000000000000000000, 0.000000000000000000 ) ) ;
#15909 = B_SPLINE_CURVE_WITH_KNOTS ( 'NONE', 3,
 ( #16866, #4390, #11480, #3006, #14897, #1164, #16753, #4278, #18349, #15122, #13402, #20426, #16637, #9763, #22028, #8051 ),
 .UNSPECIFIED., .F., .F.,
 ( 4, 2, 2, 2, 2, 2, 2, 4 ),
 ( 8.673617379884034509E-19, 0.003169695113379726766, 0.006339390226759453531, 0.007924237783449316480, 0.008716661561794248822, 0.009509085340139179429, 0.01109393289682905105, 0.01267878045351892267 ),
 .UNSPECIFIED. ) ;
#15910 = DIRECTION ( 'NONE',  ( 6.505213034913038160E-19, 3.903127820947822896E-18, 1.000000000000000000 ) ) ;
#15911 = ORIENTED_EDGE ( 'NONE', *, *, #8605, .T. ) ;
#15912 = CARTESIAN_POINT ( 'NONE',  ( -21.65063509461084834, 12.49999999999965006, 3.000000000000023537 ) ) ;
#15913 = CARTESIAN_POINT ( 'NONE',  ( -11.68090480754633553, 3.765577839755393619, -57.90797000640142045 ) ) ;
#15914 = ORIENTED_EDGE ( 'NONE', *, *, #364, .T. ) ;
#15915 = CARTESIAN_POINT ( 'NONE',  ( 0.000000000000000000, -40.00000000000000000, 0.000000000000000000 ) ) ;
#15916 = EDGE_CURVE ( 'NONE', #12233, #8676, #1719, .T. ) ;
#15917 = DIRECTION ( 'NONE',  ( -1.000000000000000000, -1.208970125616060101E-17, 6.505213034913038160E-19 ) ) ;
#15918 = VECTOR ( 'NONE', #12328, 1000.000000000000000 ) ;
#15919 = LINE ( 'NONE', #22611, #18110 ) ;
#15920 = EDGE_CURVE ( 'NONE', #19146, #12705, #15954, .T. ) ;
#15921 = FACE_OUTER_BOUND ( 'NONE', #2719, .T. ) ;
#15922 = VERTEX_POINT ( 'NONE', #15681 ) ;
#15923 = DIRECTION ( 'NONE',  ( 1.000000000000000000, 0.000000000000000000, 0.000000000000000000 ) ) ;
#15924 = CARTESIAN_POINT ( 'NONE',  ( -12.24744603029287937, 40.00000000000000000, -54.43639671998464991 ) ) ;
#15925 = DIRECTION ( 'NONE',  ( 0.000000000000000000, 0.000000000000000000, 1.000000000000000000 ) ) ;
#15926 = EDGE_LOOP ( 'NONE', ( #15634, #1772 ) ) ;
#15927 = LINE ( 'NONE', #21218, #12001 ) ;
#15928 = ADVANCED_FACE ( 'NONE', ( #5825 ), #9012, .T. ) ;
#15929 = DIRECTION ( 'NONE',  ( -0.000000000000000000, -1.000000000000000000, -0.000000000000000000 ) ) ;
#15930 = CARTESIAN_POINT ( 'NONE',  ( 9.952189117650862116, 40.00000000000000000, -53.64426396172072486 ) ) ;
#15931 = AXIS2_PLACEMENT_3D ( 'NONE', #4602, #11582, #6763 ) ;
#15932 = AXIS2_PLACEMENT_3D ( 'NONE', #6701, #6593, #10014 ) ;
#15933 = CIRCLE ( 'NONE', #4606, 58.99999999999702283 ) ;
#15934 = EDGE_LOOP ( 'NONE', ( #1544, #10046, #15346, #3931 ) ) ;
#15935 = CIRCLE ( 'NONE', #6078, 2.500000000000002220 ) ;
#15936 = VERTEX_POINT ( 'NONE', #20968 ) ;
#15937 = ORIENTED_EDGE ( 'NONE', *, *, #1069, .F. ) ;
#15938 = SHAPE_REPRESENTATION_RELATIONSHIP ( 'NONE' , 'NONE' ,  #21420, #6071 ) ;
#15939 = ORIENTED_EDGE ( 'NONE', *, *, #7889, .F. ) ;
#15940 = CARTESIAN_POINT ( 'NONE',  ( 42.50000000000000711, -9.600000000000001421, -47.50000000000000000 ) ) ;
#15941 = CARTESIAN_POINT ( 'NONE',  ( -1.387778780781445676E-14, 20.00000000000000000, 60.00200000000000244 ) ) ;
#15942 = EDGE_CURVE ( 'NONE', #8817, #18120, #12244, .T. ) ;
#15943 = CARTESIAN_POINT ( 'NONE',  ( 0.7361814224980237631, 39.99998183296705179, -49.30708964234285219 ) ) ;
#15944 = CARTESIAN_POINT ( 'NONE',  ( 9.272092376743565012, 39.99999999999999289, 53.43088570351475397 ) ) ;
#15945 = ORIENTED_EDGE ( 'NONE', *, *, #10291, .T. ) ;
#15946 = DIRECTION ( 'NONE',  ( -1.000000000000000000, -2.650195244404477958E-14, 0.000000000000000000 ) ) ;
#15947 = LINE ( 'NONE', #21127, #13556 ) ;
#15948 = EDGE_LOOP ( 'NONE', ( #1196, #1760, #20851, #17611 ) ) ;
#15949 = AXIS2_PLACEMENT_3D ( 'NONE', #13231, #22089, #6380 ) ;
#15950 = CIRCLE ( 'NONE', #15592, 31.50000000000001421 ) ;
#15951 = CARTESIAN_POINT ( 'NONE',  ( 0.2891450487059649133, -0.01224742503970683433, 48.63032622729384258 ) ) ;
#15952 = VECTOR ( 'NONE', #7233, 1000.000000000000000 ) ;
#15953 = CARTESIAN_POINT ( 'NONE',  ( 6.102098042870833506E-15, -2.522175986002989312, 47.48283745780745591 ) ) ;
#15954 = CIRCLE ( 'NONE', #21088, 2.099999999999997868 ) ;
#15955 = FACE_OUTER_BOUND ( 'NONE', #1942, .T. ) ;
#15956 = ORIENTED_EDGE ( 'NONE', *, *, #3763, .T. ) ;
#15957 = ORIENTED_EDGE ( 'NONE', *, *, #4434, .T. ) ;
#15958 = DIRECTION ( 'NONE',  ( 0.000000000000000000, 0.000000000000000000, -1.000000000000000000 ) ) ;
#15959 = CARTESIAN_POINT ( 'NONE',  ( -7.538461658765283957, 38.52939893239184954, 55.92178727523601367 ) ) ;
#15960 = DIRECTION ( 'NONE',  ( 1.296372316667914327E-16, 1.000000000000000000, -0.000000000000000000 ) ) ;
#15961 = VECTOR ( 'NONE', #21622, 1000.000000000000000 ) ;
#15962 = CARTESIAN_POINT ( 'NONE',  ( 8.687723243037263288, 39.99999999999999289, -53.22563606164203520 ) ) ;
#15963 = CARTESIAN_POINT ( 'NONE',  ( 22.38794582965086022, 21.29119307984318255, 58.65949541090324715 ) ) ;
#15964 = CARTESIAN_POINT ( 'NONE',  ( 90.00000000000000000, 40.00000000000000711, 2.524999999999998579 ) ) ;
#15965 = DIRECTION ( 'NONE',  ( 6.505213034913038160E-19, 3.903127820947822896E-18, 1.000000000000000000 ) ) ;
#15966 = B_SPLINE_CURVE_WITH_KNOTS ( 'NONE', 3,
 ( #22155, #6452, #11938, #18714, #17206, #1520 ),
 .UNSPECIFIED., .F., .F.,
 ( 4, 2, 4 ),
 ( 1.748223473168675632E-18, 0.004604358499702457599, 0.009208716999404913464 ),
 .UNSPECIFIED. ) ;
#15967 = AXIS2_PLACEMENT_3D ( 'NONE', #4595, #18907, #22122 ) ;
#15969 = VERTEX_POINT ( 'NONE', #672 ) ;
#15968 = EDGE_CURVE ( 'NONE', #20188, #159, #13021, .T. ) ;
#15970 = VERTEX_POINT ( 'NONE', #19813 ) ;
#15971 = ORIENTED_EDGE ( 'NONE', *, *, #19770, .F. ) ;
#15972 = ORIENTED_EDGE ( 'NONE', *, *, #4022, .F. ) ;
#15973 = FACE_OUTER_BOUND ( 'NONE', #7441, .T. ) ;
#15974 = EDGE_CURVE ( 'NONE', #15849, #10226, #14849, .T. ) ;
#15975 = AXIS2_PLACEMENT_3D ( 'NONE', #9381, #17964, #20992 ) ;
#15976 = CARTESIAN_POINT ( 'NONE',  ( 2.775557561562891351E-14, -2.775557561562891351E-14, 2.999999999999995559 ) ) ;
#15977 = ADVANCED_FACE ( 'NONE', ( #14636 ), #2393, .T. ) ;
#15978 = DIRECTION ( 'NONE',  ( -6.505213034913038160E-19, -3.903127820947822896E-18, -1.000000000000000000 ) ) ;
#15979 = DIRECTION ( 'NONE',  ( 6.505213034913038160E-19, 3.903127820947822896E-18, 1.000000000000000000 ) ) ;
#15980 = DIRECTION ( 'NONE',  ( -0.000000000000000000, -0.000000000000000000, 1.000000000000000000 ) ) ;
#15981 = CARTESIAN_POINT ( 'NONE',  ( 0.8008155648455618225, 39.99628551735307980, 49.34729276519122720 ) ) ;
#15982 = ORIENTED_EDGE ( 'NONE', *, *, #21865, .F. ) ;
#15983 = DIRECTION ( 'NONE',  ( 0.000000000000000000, -0.000000000000000000, -1.000000000000000000 ) ) ;
#15984 = CIRCLE ( 'NONE', #6126, 31.50000000000001421 ) ;
#15985 = CARTESIAN_POINT ( 'NONE',  ( 42.50000000000000711, -12.00000000000012434, -47.50000000000000000 ) ) ;
#15986 = FACE_OUTER_BOUND ( 'NONE', #5651, .T. ) ;
#15987 = DIRECTION ( 'NONE',  ( 1.000000000000000000, 0.000000000000000000, 0.000000000000000000 ) ) ;
#15988 = CIRCLE ( 'NONE', #6127, 2.525000000000110489 ) ;
#15989 = CARTESIAN_POINT ( 'NONE',  ( 2.347663744114436568, 31.41239365194195443, -2.999999999999971578 ) ) ;
#15990 = EDGE_CURVE ( 'NONE', #16547, #14529, #21777, .T. ) ;
#15991 = B_SPLINE_CURVE_WITH_KNOTS ( 'NONE', 3,
 ( #19311, #19426, #269, #3726, #12192, #10677, #5438, #9103, #386, #1995, #9206, #17460, #14346, #13901, #12513, #15959, #20917, #12308 ),
 .UNSPECIFIED., .F., .F.,
 ( 4, 2, 2, 2, 2, 2, 2, 2, 4 ),
 ( -3.543127106788223826E-05, 0.0006851204654911835761, 0.001405672202050249533, 0.002846775675168380579, 0.005728982621404643538, 0.007170086094522767212, 0.008611189567640890885, 0.01005229304075901629, 0.01149339651387713823 ),
 .UNSPECIFIED. ) ;
#15992 =( BOUNDED_SURFACE ( )  B_SPLINE_SURFACE ( 3, 2, ( 
 ( #12930, #2646, #11222 ),
 ( #6412, #16498, #13378 ),
 ( #9618, #21778, #16611 ),
 ( #917, #13716, #8467 ),
 ( #3433, #5043, #12238 ),
 ( #8242, #8359, #11897 ),
 ( #16944, #15328, #15213 ),
 ( #11781, #22232, #3209 ),
 ( #20735, #6531, #13490 ),
 ( #22348, #18902, #17276 ),
 ( #6637, #20507, #13838 ),
 ( #6752, #12024, #4922 ),
 ( #10175, #19018, #10394 ),
 ( #3329, #4814, #1590 ),
 ( #15674, #13940, #1482 ),
 ( #6870, #18783, #13597 ),
 ( #20609, #10286, #15436 ),
 ( #15552, #8696, #3088 ),
 ( #8579, #1248, #12038 ),
 ( #6984, #19243, #17168 ),
 ( #22580, #20855, #9952 ),
 ( #22458, #5159, #10058 ),
 ( #17057, #20961, #12131 ),
 ( #19127, #17393, #1364 ),
 ( #1712, #5262, #17734 ),
 ( #2161, #15780, #10971 ),
 ( #17963, #12565, #21405 ),
 ( #5584, #4002, #19362 ),
 ( #14048, #16009, #16235 ),
 ( #21523, #10852, #200 ),
 ( #9029, #19576, #7194 ),
 ( #2267, #9250, #12350 ),
 ( #5704, #10510, #19699 ),
 ( #21068, #5824, #19465 ),
 ( #12792, #90, #3885 ),
 ( #3553, #1828, #14164 ),
 ( #12677, #2041, #545 ),
 ( #7541, #14513, #17515 ) ),
 .UNSPECIFIED., .F., .F., .F. ) 
 B_SPLINE_SURFACE_WITH_KNOTS ( ( 4, 2, 2, 2, 2, 2, 2, 2, 2, 2, 2, 2, 2, 2, 2, 2, 2, 2, 4 ),
 ( 3, 3 ),
 ( -1.734723475976807094E-18, 0.005809515383400554699, 0.008714273075100833349, 0.01161903076680111113, 0.01452378845850138891, 0.01742854615020166670, 0.02033330384190194795, 0.02178568268775208511, 0.02323806153360222573, 0.02614281922530250352, 0.02759519807115264414, 0.02904757691700278477, 0.03485709230040334033, 0.03630947114625347749, 0.03776184999210362159, 0.04066660768380389590, 0.04211898652965403306, 0.04357136537550417021, 0.04647612306720445147 ),
 ( 0.000000000000000000, 1.000000000000000000 ),
 .UNSPECIFIED. ) 
 GEOMETRIC_REPRESENTATION_ITEM ( )  RATIONAL_B_SPLINE_SURFACE ( (
 ( 1.000000000000000000, 0.6290213284793358950, 1.000000000000000000),
 ( 1.000000000000000000, 0.6248939334222242126, 1.000000000000000000),
 ( 1.000000000000000000, 0.6231525367047958675, 1.000000000000000000),
 ( 1.000000000000000000, 0.6225790212150504876, 1.000000000000000000),
 ( 1.000000000000000000, 0.6227321005840230628, 1.000000000000000000),
 ( 1.000000000000000000, 0.6234255931483526636, 1.000000000000000000),
 ( 1.000000000000000000, 0.6239617638515310150, 1.000000000000000000),
 ( 1.000000000000000000, 0.6251439415235403585, 1.000000000000000000),
 ( 1.000000000000000000, 0.6257917911443122705, 1.000000000000000000),
 ( 1.000000000000000000, 0.6269741839743763201, 1.000000000000000000),
 ( 1.000000000000000000, 0.6274966600224941571, 1.000000000000000000),
 ( 1.000000000000000000, 0.6282667852389499652, 1.000000000000000000),
 ( 1.000000000000000000, 0.6285148504006200509, 1.000000000000000000),
 ( 1.000000000000000000, 0.6286307432043518606, 1.000000000000000000),
 ( 1.000000000000000000, 0.6286269973793257027, 1.000000000000000000),
 ( 1.000000000000000000, 0.6285335994514142932, 1.000000000000000000),
 ( 1.000000000000000000, 0.6284444584878937645, 1.000000000000000000),
 ( 1.000000000000000000, 0.6280613430733316127, 1.000000000000000000),
 ( 1.000000000000000000, 0.6276496514148416361, 1.000000000000000000),
 ( 1.000000000000000000, 0.6268798492417411161, 1.000000000000000000),
 ( 1.000000000000000000, 0.6265983628751120582, 1.000000000000000000),
 ( 1.000000000000000000, 0.6260058463377161653, 1.000000000000000000),
 ( 1.000000000000000000, 0.6256937179553445638, 1.000000000000000000),
 ( 1.000000000000000000, 0.6241358698944529104, 1.000000000000000000),
 ( 1.000000000000000000, 0.6228888902097833302, 1.000000000000000000),
 ( 1.000000000000000000, 0.6226627606242427504, 1.000000000000000000),
 ( 1.000000000000000000, 0.6226866229701819577, 1.000000000000000000),
 ( 1.000000000000000000, 0.6229108014427029438, 1.000000000000000000),
 ( 1.000000000000000000, 0.6231102808941239024, 1.000000000000000000),
 ( 1.000000000000000000, 0.6240167787609354200, 1.000000000000000000),
 ( 1.000000000000000000, 0.6250322308934098681, 1.000000000000000000),
 ( 1.000000000000000000, 0.6273487183755138696, 1.000000000000000000),
 ( 1.000000000000000000, 0.6282530044593889196, 1.000000000000000000),
 ( 1.000000000000000000, 0.6303541273113951737, 1.000000000000000000),
 ( 1.000000000000000000, 0.6315549423243406180, 1.000000000000000000),
 ( 1.000000000000000000, 0.6356032421438199131, 1.000000000000000000),
 ( 1.000000000000000000, 0.6388921020274636042, 1.000000000000000000),
 ( 1.000000000000000000, 0.6428092274089118874, 1.000000000000000000) ) ) 
 REPRESENTATION_ITEM ( '' )  SURFACE ( )  );
#15993 = VECTOR ( 'NONE', #3571, 1000.000000000000000 ) ;
#15994 = AXIS2_PLACEMENT_3D ( 'NONE', #15941, #254, #21231 ) ;
#15995 = CARTESIAN_POINT ( 'NONE',  ( -1.387778780781445676E-14, 20.00000000000000000, -105.0020000000000095 ) ) ;
#15996 = ADVANCED_FACE ( 'NONE', ( #17968 ), #19920, .F. ) ;
#15997 = VERTEX_POINT ( 'NONE', #10858 ) ;
#15998 = AXIS2_PLACEMENT_3D ( 'NONE', #10911, #14683, #10788 ) ;
#15999 = ORIENTED_EDGE ( 'NONE', *, *, #10953, .T. ) ;
#16000 = AXIS2_PLACEMENT_3D ( 'NONE', #13467, #20830, #22208 ) ;
#16001 = CIRCLE ( 'NONE', #13446, 1.000000000000000888 ) ;
#16002 = VERTEX_POINT ( 'NONE', #10980 ) ;
#16003 = CARTESIAN_POINT ( 'NONE',  ( 5.551115123125782702E-14, -1.387778780781445676E-13, -5.749999999999949374 ) ) ;
#16004 = LINE ( 'NONE', #12232, #2860 ) ;
#16005 = CARTESIAN_POINT ( 'NONE',  ( 5.551115123125782702E-14, -1.387778780781445676E-13, -5.749999999999949374 ) ) ;
#16006 = VECTOR ( 'NONE', #18129, 1000.000000000000000 ) ;
#16007 = CYLINDRICAL_SURFACE ( 'NONE', #18532, 36.76383501243555685 ) ;
#16008 = CARTESIAN_POINT ( 'NONE',  ( -19.59430950039320152, 28.88846368933331732, -2.999999999999999112 ) ) ;
#16009 = CARTESIAN_POINT ( 'NONE',  ( -15.13173276104699916, 33.09480349269330901, -56.64473394289596797 ) ) ;
#16010 = CARTESIAN_POINT ( 'NONE',  ( 21.05198877411804048, -30.13956425491232238, 2.800654218530485018 ) ) ;
#16011 = AXIS2_PLACEMENT_3D ( 'NONE', #17056, #13837, #20734 ) ;
#16012 = ADVANCED_FACE ( 'NONE', ( #7321 ), #19581, .F. ) ;
#16013 = EDGE_LOOP ( 'NONE', ( #20647, #9304, #1327, #420, #1896, #13169 ) ) ;
#16014 = CARTESIAN_POINT ( 'NONE',  ( -23.74488952252751162, 25.58633464742629471, -2.999999999999971578 ) ) ;
#16015 = AXIS2_PLACEMENT_3D ( 'NONE', #4773, #11631, #6702 ) ;
#16016 = FACE_OUTER_BOUND ( 'NONE', #7503, .T. ) ;
#16017 = CARTESIAN_POINT ( 'NONE',  ( 0.000000000000000000, 9.999999999999998224, 3.399999999999995026 ) ) ;
#16018 = CARTESIAN_POINT ( 'NONE',  ( 37.09999999999980957, 28.00000000000000000, 54.99999999999922551 ) ) ;
#16019 = ORIENTED_EDGE ( 'NONE', *, *, #16660, .F. ) ;
#16020 = FACE_OUTER_BOUND ( 'NONE', #19650, .T. ) ;
#16021 = PLANE ( 'NONE',  #16332 ) ;
#16022 = EDGE_CURVE ( 'NONE', #14245, #6975, #16360, .T. ) ;
#16023 = CARTESIAN_POINT ( 'NONE',  ( -21.05198877411806890, 30.13956425491229396, 2.800654218530481465 ) ) ;
#16024 = AXIS2_PLACEMENT_3D ( 'NONE', #18081, #21762, #18421 ) ;
#16025 = ORIENTED_EDGE ( 'NONE', *, *, #15325, .T. ) ;
#16026 = AXIS2_PLACEMENT_3D ( 'NONE', #20458, #7971, #8188 ) ;
#16027 = CIRCLE ( 'NONE', #12746, 31.50000000000000711 ) ;
#16028 = ADVANCED_FACE ( 'NONE', ( #11202 ), #10057, .T. ) ;
#16029 = AXIS2_PLACEMENT_3D ( 'NONE', #5954, #19828, #4130 ) ;
#16030 = ORIENTED_EDGE ( 'NONE', *, *, #19848, .T. ) ;
#16031 = CARTESIAN_POINT ( 'NONE',  ( 0.2573513720701691709, 39.99960945924427591, -48.93325617798620897 ) ) ;
#16032 = DIRECTION ( 'NONE',  ( -1.000000000000000000, 0.000000000000000000, 0.000000000000000000 ) ) ;
#16033 = CARTESIAN_POINT ( 'NONE',  ( -10.30713387248692037, 2.842164160680662466, 57.27491564205614338 ) ) ;
#16034 = CARTESIAN_POINT ( 'NONE',  ( -28.07080038625074536, -14.29266125237915830, -6.999999999999992006 ) ) ;
#16035 = ORIENTED_EDGE ( 'NONE', *, *, #14188, .T. ) ;
#16036 = CARTESIAN_POINT ( 'NONE',  ( -35.00000000000000000, 17.00000000000000000, 41.00000000000002132 ) ) ;
#16037 = EDGE_CURVE ( 'NONE', #5360, #16994, #14286, .T. ) ;
#16038 = CARTESIAN_POINT ( 'NONE',  ( -8.687717822783543653, 39.99999999999999289, 53.22563407722359585 ) ) ;
#16039 = VERTEX_POINT ( 'NONE', #7662 ) ;
#16040 = DIRECTION ( 'NONE',  ( -0.000000000000000000, -1.000000000000000000, -0.000000000000000000 ) ) ;
#16041 = CARTESIAN_POINT ( 'NONE',  ( 22.25047517524400931, 22.91581175091616274, -58.62998360803280207 ) ) ;
#16042 = DIRECTION ( 'NONE',  ( 0.000000000000000000, 0.000000000000000000, -1.000000000000000000 ) ) ;
#16043 = EDGE_CURVE ( 'NONE', #13884, #9581, #2628, .T. ) ;
#16044 = CIRCLE ( 'NONE', #6909, 2.525000000000110489 ) ;
#16045 = VERTEX_POINT ( 'NONE', #4348 ) ;
#16046 = CARTESIAN_POINT ( 'NONE',  ( -9.689843208404443686, 39.33333333333332860, 54.54983754392751649 ) ) ;
#16047 = CARTESIAN_POINT ( 'NONE',  ( -34.99999999999980815, 28.00000000000000000, 54.99999999999922551 ) ) ;
#16048 = VECTOR ( 'NONE', #8385, 1000.000000000000000 ) ;
#16049 = CARTESIAN_POINT ( 'NONE',  ( -4.589694866125703321, 39.86882942939622154, -51.95767931116155580 ) ) ;
#16050 = VERTEX_POINT ( 'NONE', #787 ) ;
#16051 = CARTESIAN_POINT ( 'NONE',  ( -35.00000000000000000, 14.00000000000000000, 2.365113165210053967E-14 ) ) ;
#16052 = CARTESIAN_POINT ( 'NONE',  ( -35.00000000000000000, 0.000000000000000000, 1.387778780781445676E-14 ) ) ;
#16054 = ADVANCED_FACE ( 'NONE', ( #552, #18077 ), #12684, .F. ) ;
#16053 = ORIENTED_EDGE ( 'NONE', *, *, #17247, .T. ) ;
#16055 = EDGE_CURVE ( 'NONE', #8182, #10164, #9753, .T. ) ;
#16056 = ORIENTED_EDGE ( 'NONE', *, *, #7859, .F. ) ;
#16057 = CIRCLE ( 'NONE', #2536, 0.9999999999999974465 ) ;
#16058 = EDGE_LOOP ( 'NONE', ( #6154, #4248, #4188, #2425 ) ) ;
#16059 = AXIS2_PLACEMENT_3D ( 'NONE', #11482, #21809, #8270 ) ;
#16060 =( NAMED_UNIT ( * ) PLANE_ANGLE_UNIT ( ) SI_UNIT ( $, .RADIAN. ) );
#16061 = ORIENTED_EDGE ( 'NONE', *, *, #6995, .T. ) ;
#16062 = DIRECTION ( 'NONE',  ( -0.000000000000000000, -1.000000000000000000, -0.000000000000000000 ) ) ;
#16063 = CARTESIAN_POINT ( 'NONE',  ( -89.99999999999701572, 0.000000000000000000, -3.012171160963566127E-14 ) ) ;
#16064 = DIRECTION ( 'NONE',  ( 0.000000000000000000, 0.000000000000000000, -1.000000000000000000 ) ) ;
#16065 = CARTESIAN_POINT ( 'NONE',  ( 6.975411441287900693, 40.00000000000000000, 52.53649951873629931 ) ) ;
#16066 = EDGE_CURVE ( 'NONE', #15217, #17930, #12977, .T. ) ;
#16067 = ORIENTED_EDGE ( 'NONE', *, *, #20235, .F. ) ;
#16068 = DIRECTION ( 'NONE',  ( -1.000000000000000000, 0.000000000000000000, 0.000000000000000000 ) ) ;
#16069 = LINE ( 'NONE', #19861, #272 ) ;
#16070 = VERTEX_POINT ( 'NONE', #5937 ) ;
#16071 = CARTESIAN_POINT ( 'NONE',  ( 35.00000000000000000, 25.00000000000000000, 17.00000000000002487 ) ) ;
#16072 = CARTESIAN_POINT ( 'NONE',  ( -20.89754528720910898, 28.21939688025628357, -58.32034131438403080 ) ) ;
#16073 = DIRECTION ( 'NONE',  ( -0.000000000000000000, 1.000000000000000000, -0.000000000000000000 ) ) ;
#16074 = ORIENTED_EDGE ( 'NONE', *, *, #4292, .F. ) ;
#16075 = CARTESIAN_POINT ( 'NONE',  ( 1.438414332627902414, -1.268869129817755681, 49.24051559643875464 ) ) ;
#16076 = ORIENTED_EDGE ( 'NONE', *, *, #8746, .T. ) ;
#16077 = CARTESIAN_POINT ( 'NONE',  ( 35.99819890246980236, -7.463862311151397755, -2.800654218530467698 ) ) ;
#16078 = DIRECTION ( 'NONE',  ( -6.505213034913038160E-19, -3.903127820947822896E-18, -1.000000000000000000 ) ) ;
#16079 = CARTESIAN_POINT ( 'NONE',  ( 35.00000000000001421, 0.000000000000000000, 1.540743955509788682E-30 ) ) ;
#16080 = ORIENTED_EDGE ( 'NONE', *, *, #7997, .F. ) ;
#16081 = CIRCLE ( 'NONE', #1085, 2.499999999999998668 ) ;
#16082 = CARTESIAN_POINT ( 'NONE',  ( 21.32169069720648835, 26.98977702688153357, 58.42023943869689617 ) ) ;
#16083 = LINE ( 'NONE', #12976, #5579 ) ;
#16084 = FACE_BOUND ( 'NONE', #7674, .T. ) ;
#16086 = EDGE_CURVE ( 'NONE', #19434, #8181, #2273, .T. ) ;
#16085 = ORIENTED_EDGE ( 'NONE', *, *, #14483, .F. ) ;
#16087 = CIRCLE ( 'NONE', #20865, 59.99999999999703704 ) ;
#16088 = ORIENTED_EDGE ( 'NONE', *, *, #11468, .T. ) ;
#16089 = ORIENTED_EDGE ( 'NONE', *, *, #9396, .T. ) ;
#16090 = ORIENTED_EDGE ( 'NONE', *, *, #9588, .F. ) ;
#16091 = CARTESIAN_POINT ( 'NONE',  ( -42.50000000000000711, -12.00000000000012434, -47.50000000000000000 ) ) ;
#16092 = FACE_OUTER_BOUND ( 'NONE', #20714, .T. ) ;
#16093 = DIRECTION ( 'NONE',  ( -1.000000000000000000, 0.000000000000000000, 0.000000000000000000 ) ) ;
#16094 = VECTOR ( 'NONE', #11766, 1000.000000000000000 ) ;
#16095 = EDGE_CURVE ( 'NONE', #8847, #10947, #11167, .T. ) ;
#16096 = CARTESIAN_POINT ( 'NONE',  ( 7.505578006071305985, 1.461761173326671104, 55.63523492903841117 ) ) ;
#16097 = CARTESIAN_POINT ( 'NONE',  ( -0.003185071962412873176, 13.00000169078104051, 8.999999436406458386 ) ) ;
#16098 = EDGE_LOOP ( 'NONE', ( #11157, #18726, #10135, #2285 ) ) ;
#16099 = CYLINDRICAL_SURFACE ( 'NONE', #18516, 2.099999999999990763 ) ;
#16100 = CARTESIAN_POINT ( 'NONE',  ( 35.00000000000000000, 39.00000000000000711, 4.258610482196280173E-15 ) ) ;
#16101 = CARTESIAN_POINT ( 'NONE',  ( 14.99999999999998579, 20.00000000000000355, -101.0000000000000284 ) ) ;
#16102 = DIRECTION ( 'NONE',  ( 0.000000000000000000, -0.000000000000000000, 1.000000000000000000 ) ) ;
#16103 = ADVANCED_FACE ( 'NONE', ( #11085 ), #21991, .T. ) ;
#16104 = AXIS2_PLACEMENT_3D ( 'NONE', #16005, #17512, #14389 ) ;
#16105 = CARTESIAN_POINT ( 'NONE',  ( -25.00000000000000000, 20.00000000000000000, 6.487780019669002523E-15 ) ) ;
#16106 = EDGE_CURVE ( 'NONE', #10374, #19286, #22655, .T. ) ;
#16107 = DIRECTION ( 'NONE',  ( 6.505213034913038160E-19, 3.903127820947822896E-18, 1.000000000000000000 ) ) ;
#16108 = LINE ( 'NONE', #12664, #18542 ) ;
#16109 = ORIENTED_EDGE ( 'NONE', *, *, #9451, .T. ) ;
#16110 = ORIENTED_EDGE ( 'NONE', *, *, #14065, .T. ) ;
#16111 = EDGE_LOOP ( 'NONE', ( #21302, #936, #16540, #3288 ) ) ;
#16112 = LINE ( 'NONE', #18182, #512 ) ;
#16113 = AXIS2_PLACEMENT_3D ( 'NONE', #6810, #20790, #12182 ) ;
#16114 = DIRECTION ( 'NONE',  ( 6.505213034913038160E-19, 3.903127820947822896E-18, 1.000000000000000000 ) ) ;
#16115 = CARTESIAN_POINT ( 'NONE',  ( 1.110223024625156540E-13, -5.551115123125782702E-14, -6.999999999999950262 ) ) ;
#16116 = CARTESIAN_POINT ( 'NONE',  ( 13.00000000000000178, -20.00000000000000000, -11.32475165290605901 ) ) ;
#16117 = EDGE_CURVE ( 'NONE', #10716, #626, #14806, .T. ) ;
#16118 = DIRECTION ( 'NONE',  ( -0.000000000000000000, -0.000000000000000000, 1.000000000000000000 ) ) ;
#16119 = CARTESIAN_POINT ( 'NONE',  ( -10.01331137436150520, 34.09180625983466939, -3.000000000000018208 ) ) ;
#16120 = ORIENTED_EDGE ( 'NONE', *, *, #4936, .T. ) ;
#16121 = DIRECTION ( 'NONE',  ( 0.000000000000000000, -1.000000000000000000, 0.000000000000000000 ) ) ;
#16122 = CARTESIAN_POINT ( 'NONE',  ( -5.666159602074104740, 39.18446031140960883, -54.55708815122285671 ) ) ;
#16123 = DIRECTION ( 'NONE',  ( 0.000000000000000000, -0.000000000000000000, -1.000000000000000000 ) ) ;
#16124 = CARTESIAN_POINT ( 'NONE',  ( 26.50842683089785368, -24.41514043009201984, -2.999999999999971578 ) ) ;
#16125 = ADVANCED_FACE ( 'NONE', ( #6174 ), #20380, .F. ) ;
#16126 = ORIENTED_EDGE ( 'NONE', *, *, #21275, .F. ) ;
#16127 = CIRCLE ( 'NONE', #4444, 59.99999999999700862 ) ;
#16128 = DIRECTION ( 'NONE',  ( 0.000000000000000000, 0.000000000000000000, -1.000000000000000000 ) ) ;
#16129 = CARTESIAN_POINT ( 'NONE',  ( -35.00000000000058265, 26.00000000000000355, -57.10000000000076170 ) ) ;
#16130 = CARTESIAN_POINT ( 'NONE',  ( 14.30046708970552061, 2.690036953684188159, -56.32185947139154791 ) ) ;
#16131 = EDGE_LOOP ( 'NONE', ( #6540, #819, #7949, #6581 ) ) ;
#16132 = CARTESIAN_POINT ( 'NONE',  ( -18.22261011550271803, -31.92986134326270076, 2.800654218530509443 ) ) ;
#16133 = AXIS2_PLACEMENT_3D ( 'NONE', #4833, #15457, #13856 ) ;
#16134 = ADVANCED_FACE ( 'NONE', ( #15076, #1228 ), #10467, .F. ) ;
#16135 = ORIENTED_EDGE ( 'NONE', *, *, #12378, .F. ) ;
#16136 = DIRECTION ( 'NONE',  ( 0.000000000000000000, 1.000000000000000000, 0.000000000000000000 ) ) ;
#16137 = CARTESIAN_POINT ( 'NONE',  ( -36.76383501243532947, -2.502178713904648213E-13, 2.800654218530498785 ) ) ;
#16138 = ORIENTED_EDGE ( 'NONE', *, *, #12816, .T. ) ;
#16139 = CARTESIAN_POINT ( 'NONE',  ( 10.50000000000024514, -2.516660498395250301, 100.0000000000000000 ) ) ;
#16140 = CARTESIAN_POINT ( 'NONE',  ( -7.364735830101260206, 40.00000000000001421, 52.70305158486502961 ) ) ;
#16141 = ORIENTED_EDGE ( 'NONE', *, *, #16512, .F. ) ;
#16142 = LINE ( 'NONE', #16266, #6541 ) ;
#16143 = EDGE_CURVE ( 'NONE', #943, #43, #2013, .T. ) ;
#16145 = EDGE_CURVE ( 'NONE', #22077, #8307, #8241, .T. ) ;
#16144 = CARTESIAN_POINT ( 'NONE',  ( -12.00937115242646591, -34.74700806321101254, -1.999999999999977573 ) ) ;
#16146 = DIRECTION ( 'NONE',  ( -1.000000000000000000, -7.117517058857148288E-15, 0.000000000000000000 ) ) ;
#16147 = LINE ( 'NONE', #7230, #5300 ) ;
#16148 = VERTEX_POINT ( 'NONE', #16825 ) ;
#16149 = FACE_OUTER_BOUND ( 'NONE', #17838, .T. ) ;
#16150 = FACE_BOUND ( 'NONE', #18148, .T. ) ;
#16151 = CARTESIAN_POINT ( 'NONE',  ( -1.943364650768838686, 39.97741567493590509, -50.18563800799666552 ) ) ;
#16152 = ORIENTED_EDGE ( 'NONE', *, *, #2893, .F. ) ;
#16153 = AXIS2_PLACEMENT_3D ( 'NONE', #1960, #2073, #19608 ) ;
#16154 = LINE ( 'NONE', #8741, #8256 ) ;
#16155 = ADVANCED_FACE ( 'NONE', ( #13238 ), #6507, .T. ) ;
#16156 = CARTESIAN_POINT ( 'NONE',  ( 31.11359284679393511, 4.918774254215746211, -2.999999999999988898 ) ) ;
#16157 = EDGE_CURVE ( 'NONE', #2785, #5375, #8593, .T. ) ;
#16158 = ORIENTED_EDGE ( 'NONE', *, *, #14498, .T. ) ;
#16159 = VERTEX_POINT ( 'NONE', #19200 ) ;
#16160 = EDGE_CURVE ( 'NONE', #9803, #14096, #6411, .T. ) ;
#16161 = ORIENTED_EDGE ( 'NONE', *, *, #4485, .T. ) ;
#16162 = VERTEX_POINT ( 'NONE', #8120 ) ;
#16163 = CARTESIAN_POINT ( 'NONE',  ( 19.99999999999999645, 20.48974789854085543, 60.62177826491085142 ) ) ;
#16164 = CARTESIAN_POINT ( 'NONE',  ( 34.99999999999980815, 40.00000000000000711, 54.99999999999922551 ) ) ;
#16165 = APPLICATION_CONTEXT ( 'automotive_design' ) ;
#16166 = AXIS2_PLACEMENT_3D ( 'NONE', #14361, #16324, #14600 ) ;
#16167 = CARTESIAN_POINT ( 'NONE',  ( 5.398828385724590895, 39.81726480423273529, -52.45277685974432558 ) ) ;
#16168 = CARTESIAN_POINT ( 'NONE',  ( 30.33632613426209801, -11.35354668330701422, -7.000000000000006217 ) ) ;
#16169 = ORIENTED_EDGE ( 'NONE', *, *, #7813, .T. ) ;
#16170 = DIRECTION ( 'NONE',  ( 0.000000000000000000, 0.000000000000000000, -1.000000000000000000 ) ) ;
#16171 = CARTESIAN_POINT ( 'NONE',  ( 28.52469787935785561, 10.00000000000000000, 4.095854054471903538 ) ) ;
#16172 = ORIENTED_EDGE ( 'NONE', *, *, #6712, .T. ) ;
#16173 = EDGE_CURVE ( 'NONE', #16276, #15473, #22098, .T. ) ;
#16174 = ADVANCED_FACE ( 'NONE', ( #2736 ), #2699, .F. ) ;
#16175 = CARTESIAN_POINT ( 'NONE',  ( -0.4182360581324739424, -0.02262178349794176369, 49.14752433807508680 ) ) ;
#16176 = EDGE_CURVE ( 'NONE', #13273, #18704, #15169, .T. ) ;
#16177 = CARTESIAN_POINT ( 'NONE',  ( -22.39119123459440530, 18.77992731964037532, -58.66020055843083014 ) ) ;
#16178 = DIRECTION ( 'NONE',  ( 1.296372316667914327E-16, 1.000000000000000000, -0.000000000000000000 ) ) ;
#16179 = ORIENTED_EDGE ( 'NONE', *, *, #7605, .T. ) ;
#16180 = DIRECTION ( 'NONE',  ( 0.000000000000000000, 0.000000000000000000, 1.000000000000000000 ) ) ;
#16181 = ORIENTED_EDGE ( 'NONE', *, *, #1917, .T. ) ;
#16182 = DIRECTION ( 'NONE',  ( 6.505213034913038160E-19, 3.903127820947822896E-18, 1.000000000000000000 ) ) ;
#16183 = CARTESIAN_POINT ( 'NONE',  ( -34.13396246814577495, 14.93538271375399695, -2.999999999999999112 ) ) ;
#16184 = EDGE_CURVE ( 'NONE', #16203, #5122, #20104, .T. ) ;
#16185 = DIRECTION ( 'NONE',  ( 6.505213034913038160E-19, 3.903127820947822896E-18, 1.000000000000000000 ) ) ;
#16186 = ORIENTED_EDGE ( 'NONE', *, *, #15397, .F. ) ;
#16187 = CARTESIAN_POINT ( 'NONE',  ( 9.750126048355683750, 40.00000000000000000, -53.58570024001794962 ) ) ;
#16188 = CARTESIAN_POINT ( 'NONE',  ( 19.34774434964850798, 25.08511355156644385, 60.46357625386934842 ) ) ;
#16189 = ADVANCED_FACE ( 'NONE', ( #7611 ), #4295, .F. ) ;
#16190 = DIRECTION ( 'NONE',  ( 6.505213034913038160E-19, 3.903127820947822896E-18, 1.000000000000000000 ) ) ;
#16191 = B_SPLINE_CURVE_WITH_KNOTS ( 'NONE', 3,
 ( #7403, #5683, #12658, #11745, #13328, #4775, #13217, #20355, #4877, #1102, #20467, #2941, #13114, #20238, #18739, #3047, #6596, #4545, #18636, #1204, #9915, #13447, #15053, #7980 ),
 .UNSPECIFIED., .F., .F.,
 ( 4, 2, 2, 2, 2, 2, 2, 2, 2, 2, 2, 4 ),
 ( 0.01913044734024341512, 0.02058416378663297658, 0.02203788023302254151, 0.02494531312580167484, 0.02639902957219124671, 0.02785274601858081858, 0.03076017891135996579, 0.03221389535774953072, 0.03366761180413910259, 0.03657504469691824633, 0.03948247758969737620, 0.04238991048247651994 ),
 .UNSPECIFIED. ) ;
#16192 = AXIS2_PLACEMENT_3D ( 'NONE', #6409, #11679, #16609 ) ;
#16193 = TOROIDAL_SURFACE ( 'NONE', #19138, 34.90673715956759082, 8.750000000000000000 ) ;
#16194 = CYLINDRICAL_SURFACE ( 'NONE', #12958, 2.999999999999999112 ) ;
#16195 = AXIS2_PLACEMENT_3D ( 'NONE', #9332, #5659, #4073 ) ;
#16196 = ORIENTED_EDGE ( 'NONE', *, *, #14488, .T. ) ;
#16197 = EDGE_LOOP ( 'NONE', ( #4510, #7764, #18119, #13554, #6690, #20621, #13508, #20430, #21238, #7699, #11388, #16258 ) ) ;
#16198 = ORIENTED_EDGE ( 'NONE', *, *, #14699, .T. ) ;
#16199 = ORIENTED_EDGE ( 'NONE', *, *, #9996, .F. ) ;
#16200 = FACE_OUTER_BOUND ( 'NONE', #3485, .T. ) ;
#16201 = DIRECTION ( 'NONE',  ( 0.000000000000000000, -1.000000000000000000, 0.000000000000000000 ) ) ;
#16202 = DIRECTION ( 'NONE',  ( -0.000000000000000000, 1.000000000000000000, -0.000000000000000000 ) ) ;
#16203 = VERTEX_POINT ( 'NONE', #14590 ) ;
#16204 = CARTESIAN_POINT ( 'NONE',  ( 35.00000000000000000, 2.142135623730931471, -59.99999999999999289 ) ) ;
#16205 = CARTESIAN_POINT ( 'NONE',  ( -32.75570538720758407, 15.02862401740787135, -6.999999999999950262 ) ) ;
#16206 = AXIS2_PLACEMENT_3D ( 'NONE', #752, #14706, #17933 ) ;
#16207 = ORIENTED_EDGE ( 'NONE', *, *, #17163, .F. ) ;
#16208 = CYLINDRICAL_SURFACE ( 'NONE', #22178, 2.499999999999995115 ) ;
#16209 = AXIS2_PLACEMENT_3D ( 'NONE', #9257, #19811, #9151 ) ;
#16210 = PRODUCT_DEFINITION_CONTEXT ( 'detailed design', #14996, 'design' ) ;
#16211 = CARTESIAN_POINT ( 'NONE',  ( -35.00000000000000000, 40.00000000000000000, 1.387778780781445676E-14 ) ) ;
#16212 = CARTESIAN_POINT ( 'NONE',  ( 2.999999999999997780, 30.00000000000000000, 8.485281374238567764 ) ) ;
#16213 = DIRECTION ( 'NONE',  ( 0.000000000000000000, 1.000000000000000000, 0.000000000000000000 ) ) ;
#16214 = AXIS2_PLACEMENT_3D ( 'NONE', #17320, #22391, #3478 ) ;
#16215 = EDGE_CURVE ( 'NONE', #2243, #4414, #3854, .T. ) ;
#16216 = EDGE_CURVE ( 'NONE', #14343, #2308, #8057, .T. ) ;
#16217 = CARTESIAN_POINT ( 'NONE',  ( -34.99999999999980815, 28.00000000000000000, 54.99999999999922551 ) ) ;
#16218 = CARTESIAN_POINT ( 'NONE',  ( -5.617777150769229344, 39.81214432327088559, 52.56494788744241475 ) ) ;
#16219 = ADVANCED_FACE ( 'NONE', ( #18369, #11152 ), #12862, .F. ) ;
#16220 = DIRECTION ( 'NONE',  ( 0.000000000000000000, 0.000000000000000000, -1.000000000000000000 ) ) ;
#16221 = EDGE_LOOP ( 'NONE', ( #5618, #9717, #12638, #16085 ) ) ;
#16222 = CIRCLE ( 'NONE', #16590, 3.999999999999998224 ) ;
#16223 = ORIENTED_EDGE ( 'NONE', *, *, #15742, .F. ) ;
#16224 = VECTOR ( 'NONE', #4012, 1000.000000000000000 ) ;
#16225 = VECTOR ( 'NONE', #11356, 1000.000000000000000 ) ;
#16226 = ORIENTED_EDGE ( 'NONE', *, *, #13579, .F. ) ;
#16227 = DIRECTION ( 'NONE',  ( 1.000000000000000000, 1.208970125616053475E-17, 0.000000000000000000 ) ) ;
#16228 = DIRECTION ( 'NONE',  ( 6.505213034913038160E-19, 3.903127820947822896E-18, 1.000000000000000000 ) ) ;
#16229 = CARTESIAN_POINT ( 'NONE',  ( -28.50000000000001421, 19.99999999999982947, -100.0000000000000000 ) ) ;
#16230 = EDGE_CURVE ( 'NONE', #19564, #9197, #2755, .T. ) ;
#16231 = DIRECTION ( 'NONE',  ( -0.1421319796954317316, 0.000000000000000000, -0.9898477157360405787 ) ) ;
#16232 = CIRCLE ( 'NONE', #13290, 19.11328065563151313 ) ;
#16233 = DIRECTION ( 'NONE',  ( 0.000000000000000000, 0.000000000000000000, -1.000000000000000000 ) ) ;
#16234 = CARTESIAN_POINT ( 'NONE',  ( -13.76051559511277134, 5.481080969678175485, 58.73291665846262077 ) ) ;
#16235 = CARTESIAN_POINT ( 'NONE',  ( -16.86064470394645909, 34.83129639055714932, -57.19330778950705962 ) ) ;
#16236 = CARTESIAN_POINT ( 'NONE',  ( -42.49999999999996447, 10.00000000000000000, -47.50000000000000711 ) ) ;
#16237 = CIRCLE ( 'NONE', #22475, 2.099999999999997868 ) ;
#16238 = EDGE_LOOP ( 'NONE', ( #20123, #3682, #17297, #14337, #7742, #1387 ) ) ;
#16239 = DIRECTION ( 'NONE',  ( 1.000000000000000000, 1.208970125616053321E-17, 0.000000000000000000 ) ) ;
#16240 = DIRECTION ( 'NONE',  ( 0.000000000000000000, -1.000000000000000000, 0.000000000000000000 ) ) ;
#16241 = CARTESIAN_POINT ( 'NONE',  ( -1.575352350797029954, 39.94051438458651404, -50.55779643183547734 ) ) ;
#16242 = CARTESIAN_POINT ( 'NONE',  ( -24.03323817228457315, 20.36304159388344104, -6.999999999999957367 ) ) ;
#16243 = FACE_OUTER_BOUND ( 'NONE', #1954, .T. ) ;
#16244 = AXIS2_PLACEMENT_3D ( 'NONE', #11577, #11350, #1255 ) ;
#16245 = ORIENTED_EDGE ( 'NONE', *, *, #4668, .T. ) ;
#16246 = DIRECTION ( 'NONE',  ( -6.505213034913038160E-19, -3.903127820947822896E-18, -1.000000000000000000 ) ) ;
#16247 = ORIENTED_EDGE ( 'NONE', *, *, #13670, .F. ) ;
#16248 = FACE_OUTER_BOUND ( 'NONE', #5870, .T. ) ;
#16249 = FACE_OUTER_BOUND ( 'NONE', #14570, .T. ) ;
#16250 = CARTESIAN_POINT ( 'NONE',  ( -34.99999999999999289, 5.000000000000000000, -3.012171160963566127E-14 ) ) ;
#16251 = B_SPLINE_CURVE_WITH_KNOTS ( 'NONE', 3,
 ( #16077, #1886, #8867, #3950 ),
 .UNSPECIFIED., .F., .F.,
 ( 4, 4 ),
 ( 9.545285766871421717E-07, 0.001900595205834707284 ),
 .UNSPECIFIED. ) ;
#16252 = AXIS2_PLACEMENT_3D ( 'NONE', #12576, #19589, #6683 ) ;
#16253 = ORIENTED_EDGE ( 'NONE', *, *, #20815, .T. ) ;
#16254 = EDGE_CURVE ( 'NONE', #5408, #12877, #7515, .T. ) ;
#16255 = LINE ( 'NONE', #564, #10023 ) ;
#16256 = FACE_OUTER_BOUND ( 'NONE', #5228, .T. ) ;
#16257 = CIRCLE ( 'NONE', #20303, 2.099999999999997868 ) ;
#16258 = ORIENTED_EDGE ( 'NONE', *, *, #4273, .T. ) ;
#16259 = FACE_OUTER_BOUND ( 'NONE', #8014, .T. ) ;
#16260 = DIRECTION ( 'NONE',  ( 0.000000000000000000, -0.000000000000000000, -1.000000000000000000 ) ) ;
#16261 = LINE ( 'NONE', #16034, #8743 ) ;
#16262 = ORIENTED_EDGE ( 'NONE', *, *, #16117, .F. ) ;
#16263 = DIRECTION ( 'NONE',  ( -0.5840452403773163104, -0.8117211080122302969, 0.000000000000000000 ) ) ;
#16264 = CARTESIAN_POINT ( 'NONE',  ( -13.56354382738803466, 2.142135623730932803, -56.03997097393685323 ) ) ;
#16265 = EDGE_LOOP ( 'NONE', ( #5173, #21213, #10359, #19795 ) ) ;
#16266 = CARTESIAN_POINT ( 'NONE',  ( 28.49999999999998224, 19.99999999999999645, 60.00099999999999767 ) ) ;
#16267 = DIRECTION ( 'NONE',  ( -0.000000000000000000, 1.000000000000000000, -0.000000000000000000 ) ) ;
#16268 = DIRECTION ( 'NONE',  ( -1.000000000000000000, 0.000000000000000000, 0.000000000000000000 ) ) ;
#16269 = DIRECTION ( 'NONE',  ( -0.000000000000000000, -0.000000000000000000, -1.000000000000000000 ) ) ;
#16270 = ORIENTED_EDGE ( 'NONE', *, *, #21564, .T. ) ;
#16271 = FACE_OUTER_BOUND ( 'NONE', #638, .T. ) ;
#16272 = AXIS2_PLACEMENT_3D ( 'NONE', #4688, #13361, #1350 ) ;
#16273 = DIRECTION ( 'NONE',  ( 6.505213034913038160E-19, 3.903127820947822896E-18, 1.000000000000000000 ) ) ;
#16274 = CARTESIAN_POINT ( 'NONE',  ( -0.2542263435710383490, 39.99961927927021321, -48.93085139008606888 ) ) ;
#16275 = AXIS2_PLACEMENT_3D ( 'NONE', #2519, #2170, #559 ) ;
#16276 = VERTEX_POINT ( 'NONE', #8071 ) ;
#16277 = CARTESIAN_POINT ( 'NONE',  ( 7.505578006071305097, 1.461761173326674434, 55.63523492903841117 ) ) ;
#16278 = ADVANCED_FACE ( 'NONE', ( #6459 ), #8507, .F. ) ;
#16279 = CARTESIAN_POINT ( 'NONE',  ( -1.387778780781445676E-14, 20.00000000000000000, -98.00000000000000000 ) ) ;
#16280 = AXIS2_PLACEMENT_3D ( 'NONE', #13535, #16985, #1293 ) ;
#16281 = EDGE_CURVE ( 'NONE', #2472, #3077, #20330, .T. ) ;
#16282 = ORIENTED_EDGE ( 'NONE', *, *, #13053, .F. ) ;
#16283 = AXIS2_PLACEMENT_3D ( 'NONE', #14279, #19364, #6871 ) ;
#16284 = VERTEX_POINT ( 'NONE', #15256 ) ;
#16285 = EDGE_LOOP ( 'NONE', ( #18201, #17151, #21125, #11809, #12755, #12087 ) ) ;
#16286 = ORIENTED_EDGE ( 'NONE', *, *, #22109, .T. ) ;
#16287 = DIRECTION ( 'NONE',  ( 0.000000000000000000, 1.000000000000000000, 0.000000000000000000 ) ) ;
#16288 = AXIS2_PLACEMENT_3D ( 'NONE', #3582, #119, #10541 ) ;
#16289 = DIRECTION ( 'NONE',  ( 6.505213034913038160E-19, 3.903127820947822896E-18, 1.000000000000000000 ) ) ;
#16290 = DIRECTION ( 'NONE',  ( 0.000000000000000000, 0.000000000000000000, 1.000000000000000000 ) ) ;
#16291 = FACE_OUTER_BOUND ( 'NONE', #8756, .T. ) ;
#16292 = VERTEX_POINT ( 'NONE', #9992 ) ;
#16293 = CARTESIAN_POINT ( 'NONE',  ( 7.094908322883203056, -35.33352588067112521, -2.999999999999999112 ) ) ;
#16294 = DIRECTION ( 'NONE',  ( 1.000000000000000000, 0.000000000000000000, 0.000000000000000000 ) ) ;
#16295 = ORIENTED_EDGE ( 'NONE', *, *, #10561, .F. ) ;
#16296 = DIRECTION ( 'NONE',  ( -0.000000000000000000, 1.000000000000000000, -0.000000000000000000 ) ) ;
#16297 = DIRECTION ( 'NONE',  ( -6.505213034913038160E-19, -3.903127820947822896E-18, -1.000000000000000000 ) ) ;
#16298 = CARTESIAN_POINT ( 'NONE',  ( 25.00000000000000000, -20.00000000000000000, 6.487780019669002523E-15 ) ) ;
#16299 = ORIENTED_EDGE ( 'NONE', *, *, #4426, .T. ) ;
#16300 = DIRECTION ( 'NONE',  ( 0.000000000000000000, -1.000000000000000000, 0.000000000000000000 ) ) ;
#16301 = ORIENTED_EDGE ( 'NONE', *, *, #1258, .F. ) ;
#16302 = CARTESIAN_POINT ( 'NONE',  ( 7.464609744079063525, 38.57206862716381579, 54.30635410445871258 ) ) ;
#16303 = TOROIDAL_SURFACE ( 'NONE', #5690, 34.90673715956759082, 8.750000000000000000 ) ;
#16304 = CARTESIAN_POINT ( 'NONE',  ( 7.505578006071305985, 1.461761173326671104, 55.63523492903841117 ) ) ;
#16305 = VECTOR ( 'NONE', #12625, 1000.000000000000000 ) ;
#16306 = CIRCLE ( 'NONE', #9364, 6.499999999999999112 ) ;
#16307 = ORIENTED_EDGE ( 'NONE', *, *, #6467, .F. ) ;
#16308 = PLANE ( 'NONE',  #18942 ) ;
#16309 = EDGE_CURVE ( 'NONE', #18373, #8376, #3502, .T. ) ;
#16310 = CARTESIAN_POINT ( 'NONE',  ( 13.83098800442548004, 37.66187182509651876, 56.14292165594093831 ) ) ;
#16311 = AXIS2_PLACEMENT_3D ( 'NONE', #7763, #7423, #21406 ) ;
#16312 = TOROIDAL_SURFACE ( 'NONE', #12282, 18.00000000000000355, 4.000000000000000000 ) ;
#16313 = CARTESIAN_POINT ( 'NONE',  ( -42.50000000000000711, -12.00000000000000000, -47.50000000000000000 ) ) ;
#16314 = EDGE_CURVE ( 'NONE', #22397, #10118, #6680, .T. ) ;
#16315 = EDGE_CURVE ( 'NONE', #18097, #21198, #9349, .T. ) ;
#16317 = EDGE_CURVE ( 'NONE', #22225, #5574, #11612, .T. ) ;
#16316 = ORIENTED_EDGE ( 'NONE', *, *, #22433, .T. ) ;
#16318 = VERTEX_POINT ( 'NONE', #6792 ) ;
#16319 = VERTEX_POINT ( 'NONE', #15140 ) ;
#16320 = CIRCLE ( 'NONE', #5355, 8.999999999999998224 ) ;
#16321 = CIRCLE ( 'NONE', #6454, 2.499999999999995115 ) ;
#16322 = AXIS2_PLACEMENT_3D ( 'NONE', #21323, #14199, #21214 ) ;
#16323 = ORIENTED_EDGE ( 'NONE', *, *, #10704, .T. ) ;
#16324 = DIRECTION ( 'NONE',  ( -6.505213034913038160E-19, -3.903127820947822896E-18, -1.000000000000000000 ) ) ;
#16325 = CARTESIAN_POINT ( 'NONE',  ( 2.602085213965210642E-15, 0.6398376396478597794, 0.000000000000000000 ) ) ;
#16326 = AXIS2_PLACEMENT_3D ( 'NONE', #16949, #16732, #22466 ) ;
#16327 = CARTESIAN_POINT ( 'NONE',  ( 8.256135806682694422, -0.3920627093389359996, -55.63523492904086254 ) ) ;
#16328 = EDGE_CURVE ( 'NONE', #8737, #6835, #17319, .T. ) ;
#16329 = EDGE_LOOP ( 'NONE', ( #10340, #2234, #21659, #19978 ) ) ;
#16330 = FACE_OUTER_BOUND ( 'NONE', #17869, .T. ) ;
#16331 = CARTESIAN_POINT ( 'NONE',  ( -6.699391982050521221, -4.821764332415714449, 49.69317737456928796 ) ) ;
#16332 = AXIS2_PLACEMENT_3D ( 'NONE', #17975, #7326, #12692 ) ;
#16333 = VERTEX_POINT ( 'NONE', #15596 ) ;
#16334 = DIRECTION ( 'NONE',  ( -0.000000000000000000, -1.000000000000000000, -0.000000000000000000 ) ) ;
#16335 = LINE ( 'NONE', #11524, #20445 ) ;
#16336 = DIRECTION ( 'NONE',  ( 1.067522139062650671E-15, 0.000000000000000000, -1.000000000000000000 ) ) ;
#16337 = LINE ( 'NONE', #17943, #10557 ) ;
#16338 = DIRECTION ( 'NONE',  ( 0.000000000000000000, 0.000000000000000000, 1.000000000000000000 ) ) ;
#16339 = TOROIDAL_SURFACE ( 'NONE', #10832, 34.90673715956759082, 8.750000000000000000 ) ;
#16340 = DIRECTION ( 'NONE',  ( -1.000000000000000000, -8.894490888754760711E-15, 0.000000000000000000 ) ) ;
#16341 = PLANE ( 'NONE',  #15848 ) ;
#16342 = DIRECTION ( 'NONE',  ( 0.000000000000000000, 0.000000000000000000, -1.000000000000000000 ) ) ;
#16343 = ORIENTED_EDGE ( 'NONE', *, *, #22508, .F. ) ;
#16344 = CIRCLE ( 'NONE', #14468, 1.000000000000000888 ) ;
#16345 = VERTEX_POINT ( 'NONE', #22500 ) ;
#16346 = ADVANCED_FACE ( 'NONE', ( #20776 ), #22159, .F. ) ;
#16347 = ORIENTED_EDGE ( 'NONE', *, *, #8075, .F. ) ;
#16348 = DIRECTION ( 'NONE',  ( -0.000000000000000000, 1.000000000000000000, -0.000000000000000000 ) ) ;
#16349 = EDGE_CURVE ( 'NONE', #12891, #7324, #11896, .T. ) ;
#16350 = FACE_OUTER_BOUND ( 'NONE', #12615, .T. ) ;
#16351 = TOROIDAL_SURFACE ( 'NONE', #14861, 34.90673715956759082, 8.750000000000000000 ) ;
#16352 = EDGE_CURVE ( 'NONE', #8568, #8737, #11548, .T. ) ;
#16353 = CARTESIAN_POINT ( 'NONE',  ( 19.99999999999998579, 20.00000000000000000, -105.0020000000000095 ) ) ;
#16354 = DIRECTION ( 'NONE',  ( 0.9898477157360405787, 0.000000000000000000, -0.1421319796954322312 ) ) ;
#16355 = CARTESIAN_POINT ( 'NONE',  ( -34.99999999999999289, 1.000000000000044187, -3.012171160963566127E-14 ) ) ;
#16356 = CARTESIAN_POINT ( 'NONE',  ( 35.00000000000000000, 40.00000000000000000, 4.258610482196280173E-15 ) ) ;
#16357 = LINE ( 'NONE', #4004, #22545 ) ;
#16358 = ORIENTED_EDGE ( 'NONE', *, *, #9608, .T. ) ;
#16359 = LINE ( 'NONE', #7661, #2551 ) ;
#16360 = LINE ( 'NONE', #19707, #916 ) ;
#16361 = CYLINDRICAL_SURFACE ( 'NONE', #21739, 4.000000000000145661 ) ;
#16362 = VERTEX_POINT ( 'NONE', #8401 ) ;
#16363 = AXIS2_PLACEMENT_3D ( 'NONE', #22145, #14793, #9977 ) ;
#16364 = ORIENTED_EDGE ( 'NONE', *, *, #15400, .F. ) ;
#16365 = DIRECTION ( 'NONE',  ( 1.000000000000000000, 0.000000000000000000, 0.000000000000000000 ) ) ;
#16366 = CIRCLE ( 'NONE', #2835, 36.76383501243555685 ) ;
#16367 = DIRECTION ( 'NONE',  ( 0.000000000000000000, -1.000000000000000000, 0.000000000000000000 ) ) ;
#16368 = AXIS2_PLACEMENT_3D ( 'NONE', #2270, #9256, #16239 ) ;
#16369 = ORIENTED_EDGE ( 'NONE', *, *, #7775, .F. ) ;
#16370 = DIRECTION ( 'NONE',  ( 6.505213034913038160E-19, 3.903127820947822896E-18, 1.000000000000000000 ) ) ;
#16371 = CONICAL_SURFACE ( 'NONE', #13796, 58.99999999999698730, 0.7853981633974447263 ) ;
#16372 = AXIS2_PLACEMENT_3D ( 'NONE', #18346, #2896, #6317 ) ;
#16373 = CARTESIAN_POINT ( 'NONE',  ( 3.608224830031758756E-13, -2.775557561562891351E-14, -4.999999999999997335 ) ) ;
#16374 = ORIENTED_EDGE ( 'NONE', *, *, #15293, .F. ) ;
#16375 = CARTESIAN_POINT ( 'NONE',  ( 0.2763232317742203015, 39.99954927670500382, -48.94786180895853533 ) ) ;
#16376 = AXIS2_PLACEMENT_3D ( 'NONE', #17514, #1827, #8810 ) ;
#16377 = DIRECTION ( 'NONE',  ( 6.505213034913038160E-19, 3.903127820947822896E-18, 1.000000000000000000 ) ) ;
#16378 = DIRECTION ( 'NONE',  ( 6.505213034913038160E-19, 3.903127820947822896E-18, 1.000000000000000000 ) ) ;
#16379 = AXIS2_PLACEMENT_3D ( 'NONE', #22676, #17255, #18875 ) ;
#16380 = EDGE_LOOP ( 'NONE', ( #1511, #14129, #20322 ) ) ;
#16381 = LINE ( 'NONE', #14869, #21682 ) ;
#16382 = DIRECTION ( 'NONE',  ( -0.000000000000000000, -0.000000000000000000, 1.000000000000000000 ) ) ;
#16383 = EDGE_LOOP ( 'NONE', ( #1865, #7512 ) ) ;
#16384 = CARTESIAN_POINT ( 'NONE',  ( -90.00000000000000000, 26.00000000000000355, 2.099999999999989875 ) ) ;
#16385 = AXIS2_PLACEMENT_3D ( 'NONE', #7309, #21287, #5578 ) ;
#16386 = CARTESIAN_POINT ( 'NONE',  ( 12.59807286780800517, 38.55590838447054836, -55.66678043528290232 ) ) ;
#16387 = CARTESIAN_POINT ( 'NONE',  ( 19.59430950039339692, -28.88846368933353759, 3.000000000000023537 ) ) ;
#16388 = EDGE_LOOP ( 'NONE', ( #2065, #6925, #11206, #9496 ) ) ;
#16389 = CARTESIAN_POINT ( 'NONE',  ( 14.99999999999998579, 20.00000000000000000, 45.82575694955838230 ) ) ;
#16390 = DIRECTION ( 'NONE',  ( 0.000000000000000000, 0.000000000000000000, 1.000000000000000000 ) ) ;
#16391 = DIRECTION ( 'NONE',  ( 0.000000000000000000, 0.000000000000000000, -1.000000000000000000 ) ) ;
#16392 = EDGE_CURVE ( 'NONE', #8904, #3548, #20656, .T. ) ;
#16393 = VERTEX_POINT ( 'NONE', #13639 ) ;
#16394 = CIRCLE ( 'NONE', #3246, 19.11328065563151668 ) ;
#16395 = CARTESIAN_POINT ( 'NONE',  ( 3.460816278822046447E-15, -1.500000000000015099, 0.000000000000000000 ) ) ;
#16396 = EDGE_CURVE ( 'NONE', #1277, #17217, #22539, .T. ) ;
#16397 = VECTOR ( 'NONE', #14626, 1000.000000000000000 ) ;
#16398 = VECTOR ( 'NONE', #12327, 1000.000000000000000 ) ;
#16399 = B_SPLINE_CURVE_WITH_KNOTS ( 'NONE', 3,
 ( #17248, #13682, #20696, #6953 ),
 .UNSPECIFIED., .F., .F.,
 ( 4, 4 ),
 ( 0.000000000000000000, 1.000000000000000000 ),
 .UNSPECIFIED. ) ;
#16400 = AXIS2_PLACEMENT_3D ( 'NONE', #4557, #11990, #15521 ) ;
#16401 = ORIENTED_EDGE ( 'NONE', *, *, #19378, .F. ) ;
#16402 = ORIENTED_EDGE ( 'NONE', *, *, #1668, .F. ) ;
#16403 = VERTEX_POINT ( 'NONE', #15481 ) ;
#16404 = ORIENTED_EDGE ( 'NONE', *, *, #5039, .T. ) ;
#16405 = CARTESIAN_POINT ( 'NONE',  ( -10.70799354677373572, 35.16985127952371215, 2.800654218530492123 ) ) ;
#16406 = FACE_OUTER_BOUND ( 'NONE', #18563, .T. ) ;
#16407 = DIRECTION ( 'NONE',  ( 0.000000000000000000, 0.000000000000000000, 1.000000000000000000 ) ) ;
#16408 = VECTOR ( 'NONE', #4412, 1000.000000000000000 ) ;
#16409 = DIRECTION ( 'NONE',  ( -1.000000000000000000, 0.000000000000000000, 0.000000000000000000 ) ) ;
#16410 = EDGE_LOOP ( 'NONE', ( #14448, #19090 ) ) ;
#16411 = CARTESIAN_POINT ( 'NONE',  ( 2.999999999999998224, 22.00000000000000000, 8.485281374238567764 ) ) ;
#16413 = CIRCLE ( 'NONE', #1791, 10.00000000000000000 ) ;
#16412 = DIRECTION ( 'NONE',  ( 0.000000000000000000, 0.000000000000000000, -1.000000000000000000 ) ) ;
#16414 = ORIENTED_EDGE ( 'NONE', *, *, #17402, .F. ) ;
#16415 = CARTESIAN_POINT ( 'NONE',  ( -35.00000000000000000, 10.00000000000000000, -40.99999999999997868 ) ) ;
#16416 = FACE_OUTER_BOUND ( 'NONE', #11498, .T. ) ;
#16417 = CIRCLE ( 'NONE', #10550, 2.000000000000001776 ) ;
#16418 = CARTESIAN_POINT ( 'NONE',  ( -35.51751788033345747, 1.011722470948090313, -3.000000000000000000 ) ) ;
#16419 = ORIENTED_EDGE ( 'NONE', *, *, #17725, .F. ) ;
#16420 = LINE ( 'NONE', #12541, #11981 ) ;
#16421 = DIRECTION ( 'NONE',  ( 0.000000000000000000, -1.000000000000000000, 0.000000000000000000 ) ) ;
#16422 = ORIENTED_EDGE ( 'NONE', *, *, #3298, .F. ) ;
#16423 = CARTESIAN_POINT ( 'NONE',  ( 0.6290164960638020553, 40.00000000000000000, 49.48738346577131608 ) ) ;
#16424 = EDGE_CURVE ( 'NONE', #9683, #22506, #8289, .T. ) ;
#16425 = CARTESIAN_POINT ( 'NONE',  ( 5.551115123125782702E-14, -1.387778780781445676E-13, -5.749999999999949374 ) ) ;
#16426 = AXIS2_PLACEMENT_3D ( 'NONE', #19485, #15910, #14072 ) ;
#16427 = CARTESIAN_POINT ( 'NONE',  ( -29.36548507648012318, -13.83143812983131404, -6.999999999999950262 ) ) ;
#16428 = ORIENTED_EDGE ( 'NONE', *, *, #2148, .T. ) ;
#16429 = DIRECTION ( 'NONE',  ( -1.000000000000000000, -1.208970125616046080E-17, 6.505213034913038160E-19 ) ) ;
#16430 = DIRECTION ( 'NONE',  ( -6.505213034913038160E-19, -3.903127820947822896E-18, -1.000000000000000000 ) ) ;
#16431 = CARTESIAN_POINT ( 'NONE',  ( 32.75570538720806724, -15.02862401740834386, -6.999999999999957367 ) ) ;
#16432 = EDGE_CURVE ( 'NONE', #6865, #18399, #22281, .T. ) ;
#16433 = DIRECTION ( 'NONE',  ( 1.000000000000000000, 1.208970125616063028E-17, 0.000000000000000000 ) ) ;
#16434 = VECTOR ( 'NONE', #19891, 1000.000000000000000 ) ;
#16435 = CIRCLE ( 'NONE', #15317, 59.99999999999700862 ) ;
#16436 = ORIENTED_EDGE ( 'NONE', *, *, #785, .T. ) ;
#16437 = ORIENTED_EDGE ( 'NONE', *, *, #18115, .F. ) ;
#16438 = EDGE_LOOP ( 'NONE', ( #12870, #11034, #13141, #22662 ) ) ;
#16439 = ORIENTED_EDGE ( 'NONE', *, *, #13692, .T. ) ;
#16440 = LINE ( 'NONE', #629, #10686 ) ;
#16441 = CARTESIAN_POINT ( 'NONE',  ( 7.310544252644470693E-15, 28.19616000222403684, 0.000000000000000000 ) ) ;
#16442 = PRODUCT_DEFINITION_SHAPE ( 'NONE', 'NONE',  #22019 ) ;
#16443 = DIRECTION ( 'NONE',  ( 0.000000000000000000, -1.000000000000000000, 0.000000000000000000 ) ) ;
#16444 = EDGE_CURVE ( 'NONE', #18060, #22660, #9715, .T. ) ;
#16445 = ORIENTED_EDGE ( 'NONE', *, *, #20711, .F. ) ;
#16446 = DIRECTION ( 'NONE',  ( 0.000000000000000000, 0.000000000000000000, 1.000000000000000000 ) ) ;
#16447 = CARTESIAN_POINT ( 'NONE',  ( 2.220446049250313081E-13, 2.775557561562891351E-14, -2.800654218530485018 ) ) ;
#16448 = AXIS2_PLACEMENT_3D ( 'NONE', #4225, #14401, #11201 ) ;
#16449 = ORIENTED_EDGE ( 'NONE', *, *, #22403, .F. ) ;
#16450 = CARTESIAN_POINT ( 'NONE',  ( -35.00000000000000000, 39.00000000000000711, 1.387778780781445676E-14 ) ) ;
#16451 = LINE ( 'NONE', #523, #9077 ) ;
#16452 = EDGE_CURVE ( 'NONE', #4044, #7032, #931, .T. ) ;
#16453 = CARTESIAN_POINT ( 'NONE',  ( 30.48934413892778750, -16.99647590252659057, 3.000000000000027089 ) ) ;
#16454 = ADVANCED_FACE ( 'NONE', ( #13760 ), #12064, .F. ) ;
#16455 = CARTESIAN_POINT ( 'NONE',  ( -34.99999999999999289, 5.000000000000000000, -3.012171160963566127E-14 ) ) ;
#16456 = DIRECTION ( 'NONE',  ( 0.000000000000000000, 0.000000000000000000, -1.000000000000000000 ) ) ;
#16457 = FACE_OUTER_BOUND ( 'NONE', #22357, .T. ) ;
#16458 = CARTESIAN_POINT ( 'NONE',  ( -4.628075497662138105, 39.46063506869889892, 53.65703709786524200 ) ) ;
#16459 = DIRECTION ( 'NONE',  ( -0.000000000000000000, -1.000000000000000000, -0.000000000000000000 ) ) ;
#16460 = ORIENTED_EDGE ( 'NONE', *, *, #6652, .T. ) ;
#16461 = ORIENTED_EDGE ( 'NONE', *, *, #11650, .F. ) ;
#16462 = CIRCLE ( 'NONE', #7676, 0.9999999999999974465 ) ;
#16463 = EDGE_CURVE ( 'NONE', #15027, #16867, #3924, .T. ) ;
#16464 = ORIENTED_EDGE ( 'NONE', *, *, #8513, .F. ) ;
#16465 = DIRECTION ( 'NONE',  ( -0.000000000000000000, 1.000000000000000000, -0.000000000000000000 ) ) ;
#16466 = EDGE_CURVE ( 'NONE', #15922, #295, #22175, .T. ) ;
#16467 = CARTESIAN_POINT ( 'NONE',  ( -3.125929443366052940, 0.2354807939734264444, -52.75540126681803343 ) ) ;
#16468 = CARTESIAN_POINT ( 'NONE',  ( 2.517875701377081388, 0.1458803431931041672, -52.33410116371747733 ) ) ;
#16469 = AXIS2_PLACEMENT_3D ( 'NONE', #16965, #13857, #5176 ) ;
#16470 = CARTESIAN_POINT ( 'NONE',  ( 9.412328935320623680E-15, -0.02544136969053066924, 50.05036128709051013 ) ) ;
#16471 = FACE_OUTER_BOUND ( 'NONE', #21666, .T. ) ;
#16472 = CARTESIAN_POINT ( 'NONE',  ( -3.630514520980234749, 39.68566286778591490, -51.94955441408608721 ) ) ;
#16473 = ADVANCED_FACE ( 'NONE', ( #17895 ), #1861, .T. ) ;
#16474 = CARTESIAN_POINT ( 'NONE',  ( 35.00000000000002132, -1.000000000000028644, -59.99999999999703704 ) ) ;
#16475 = DIRECTION ( 'NONE',  ( -1.000000000000000000, 0.000000000000000000, 0.000000000000000000 ) ) ;
#16476 = DIRECTION ( 'NONE',  ( 1.296372316667914327E-16, 1.000000000000000000, -0.000000000000000000 ) ) ;
#16477 = ORIENTED_EDGE ( 'NONE', *, *, #4917, .T. ) ;
#16478 = CARTESIAN_POINT ( 'NONE',  ( 0.000000000000000000, 29.97499999999999787, 0.000000000000000000 ) ) ;
#16479 = DIRECTION ( 'NONE',  ( 6.505213034913038160E-19, 3.903127820947822896E-18, 1.000000000000000000 ) ) ;
#16480 = DIRECTION ( 'NONE',  ( 8.659560562354932858E-17, 0.7071067811865474617, -0.7071067811865474617 ) ) ;
#16481 = CARTESIAN_POINT ( 'NONE',  ( -3.418729828831206752E-14, -25.00000000000000000, 15.99999999999970512 ) ) ;
#16482 = EDGE_CURVE ( 'NONE', #4363, #18451, #18144, .T. ) ;
#16483 = VERTEX_POINT ( 'NONE', #15712 ) ;
#16484 = DIRECTION ( 'NONE',  ( -0.000000000000000000, 1.000000000000000000, -0.000000000000000000 ) ) ;
#16485 = DIRECTION ( 'NONE',  ( 0.000000000000000000, 0.000000000000000000, 1.000000000000000000 ) ) ;
#16486 = CARTESIAN_POINT ( 'NONE',  ( 2.585597902343947566E-15, -8.251288694035734395, 0.000000000000000000 ) ) ;
#16487 = VECTOR ( 'NONE', #7974, 1000.000000000000000 ) ;
#16488 = ORIENTED_EDGE ( 'NONE', *, *, #6266, .T. ) ;
#16489 = DIRECTION ( 'NONE',  ( 6.505213034913038160E-19, 3.903127820947822896E-18, 1.000000000000000000 ) ) ;
#16490 = LINE ( 'NONE', #19013, #1356 ) ;
#16491 = ORIENTED_EDGE ( 'NONE', *, *, #19281, .T. ) ;
#16492 = CARTESIAN_POINT ( 'NONE',  ( 5.724878023121393156, 39.79387150756618752, -52.64592485981327030 ) ) ;
#16493 = CARTESIAN_POINT ( 'NONE',  ( 11.15511648635847486, 39.11609166919295433, 55.07420106208768829 ) ) ;
#16494 = ORIENTED_EDGE ( 'NONE', *, *, #12577, .T. ) ;
#16495 = DIRECTION ( 'NONE',  ( 8.659560562355143632E-17, -0.7071067811865302533, 0.7071067811865647812 ) ) ;
#16496 = CONICAL_SURFACE ( 'NONE', #14653, 2.099999999999997868, 1.029744258676652091 ) ;
#16497 = DIRECTION ( 'NONE',  ( 6.505213034913038160E-19, 3.903127820947822896E-18, 1.000000000000000000 ) ) ;
#16498 = CARTESIAN_POINT ( 'NONE',  ( -13.56209497732963953, 5.196600802657145302, -56.07847567635086961 ) ) ;
#16499 = DIRECTION ( 'NONE',  ( 8.659560562353731078E-17, 0.7071067811866457165, -0.7071067811864494290 ) ) ;
#16500 = CIRCLE ( 'NONE', #19444, 34.90673715956759082 ) ;
#16501 = CARTESIAN_POINT ( 'NONE',  ( 17.79500259159620512, 31.47514467962667695, 2.932460736555829506 ) ) ;
#16502 = ORIENTED_EDGE ( 'NONE', *, *, #1633, .T. ) ;
#16503 = LINE ( 'NONE', #4139, #17070 ) ;
#16504 = CARTESIAN_POINT ( 'NONE',  ( 25.99999999999998579, 19.99999999999999645, -100.0000000000000000 ) ) ;
#16505 = CARTESIAN_POINT ( 'NONE',  ( -0.05876574830816937850, 39.99997969038122392, -48.77966625399992040 ) ) ;
#16506 = EDGE_CURVE ( 'NONE', #1054, #13358, #21220, .T. ) ;
#16507 = VERTEX_POINT ( 'NONE', #9074 ) ;
#16508 = CARTESIAN_POINT ( 'NONE',  ( 8.219889501002811016, 1.750964516533572102, 56.08920281152157372 ) ) ;
#16509 = CARTESIAN_POINT ( 'NONE',  ( 9.165151389911692092, 40.00000000000000000, 56.36098470834080842 ) ) ;
#16510 = CARTESIAN_POINT ( 'NONE',  ( -32.83234229683724692, 11.85401191286869427, 3.000000000000002665 ) ) ;
#16511 = VECTOR ( 'NONE', #11702, 1000.000000000000000 ) ;
#16512 = EDGE_CURVE ( 'NONE', #2477, #12153, #4239, .T. ) ;
#16513 = ORIENTED_EDGE ( 'NONE', *, *, #7301, .T. ) ;
#16514 = ORIENTED_EDGE ( 'NONE', *, *, #15477, .F. ) ;
#16515 = CARTESIAN_POINT ( 'NONE',  ( 188.4503278704322042, 176.4913985053411523, -41.51622879058778892 ) ) ;
#16516 = UNCERTAINTY_MEASURE_WITH_UNIT (LENGTH_MEASURE( 1.000000000000000082E-05 ), #20740, 'distance_accuracy_value', 'NONE');
#16517 = EDGE_LOOP ( 'NONE', ( #1193, #9338, #22290, #19037 ) ) ;
#16518 = CARTESIAN_POINT ( 'NONE',  ( 13.28791054760747947, 34.95496542652811200, -58.55506233662529780 ) ) ;
#16519 = DIRECTION ( 'NONE',  ( 0.000000000000000000, 0.000000000000000000, 1.000000000000000000 ) ) ;
#16520 = CYLINDRICAL_SURFACE ( 'NONE', #14271, 2.099999999999997868 ) ;
#16521 = DIRECTION ( 'NONE',  ( 6.505213034913038160E-19, 3.903127820947822896E-18, 1.000000000000000000 ) ) ;
#16522 = DIRECTION ( 'NONE',  ( -0.7071067811865463515, 8.659560562354918067E-17, 0.7071067811865487940 ) ) ;
#16523 = VERTEX_POINT ( 'NONE', #12171 ) ;
#16524 = DIRECTION ( 'NONE',  ( -1.296372316667914327E-16, -1.000000000000000000, 0.000000000000000000 ) ) ;
#16525 = CARTESIAN_POINT ( 'NONE',  ( -32.10132595304125402, -5.074925817842023790, 3.000000000000006217 ) ) ;
#16526 = ORIENTED_EDGE ( 'NONE', *, *, #20533, .T. ) ;
#16527 = CARTESIAN_POINT ( 'NONE',  ( 2.775557561562891351E-14, 2.775557561562891351E-14, 5.750000000000001776 ) ) ;
#16528 = DIRECTION ( 'NONE',  ( 0.000000000000000000, 1.000000000000000000, 0.000000000000000000 ) ) ;
#16529 = EDGE_CURVE ( 'NONE', #8659, #9204, #16154, .T. ) ;
#16530 = AXIS2_PLACEMENT_3D ( 'NONE', #3230, #17189, #3109 ) ;
#16531 = CARTESIAN_POINT ( 'NONE',  ( 42.50000000000000711, -12.00000000000000000, -47.50000000000000000 ) ) ;
#16532 = EDGE_LOOP ( 'NONE', ( #4311, #6488, #6335, #13 ) ) ;
#16533 = FACE_OUTER_BOUND ( 'NONE', #10318, .T. ) ;
#16534 = DIRECTION ( 'NONE',  ( 1.000000000000000000, 0.000000000000000000, 0.000000000000000000 ) ) ;
#16535 = ORIENTED_EDGE ( 'NONE', *, *, #4145, .T. ) ;
#16536 = CARTESIAN_POINT ( 'NONE',  ( 4.750157590145799524, 39.43751370096379816, 52.76321277951888078 ) ) ;
#16537 = B_SPLINE_CURVE_WITH_KNOTS ( 'NONE', 3,
 ( #9198, #5990, #19418, #10669 ),
 .UNSPECIFIED., .F., .F.,
 ( 4, 4 ),
 ( 0.001893031756885520502, 0.003808480026563967110 ),
 .UNSPECIFIED. ) ;
#16538 = CARTESIAN_POINT ( 'NONE',  ( -0.8499999999999410250, -5.000000000000000000, -48.11213464397154382 ) ) ;
#16539 = CARTESIAN_POINT ( 'NONE',  ( -4.664248763237361928, 0.4975022168800966038, -53.81010167002803257 ) ) ;
#16540 = ORIENTED_EDGE ( 'NONE', *, *, #17402, .T. ) ;
#16541 = CARTESIAN_POINT ( 'NONE',  ( 13.09671971564443105, 38.20119746052611021, 55.86054988736559324 ) ) ;
#16542 = DIRECTION ( 'NONE',  ( -6.505213034913038160E-19, -3.903127820947822896E-18, -1.000000000000000000 ) ) ;
#16543 = DIRECTION ( 'NONE',  ( -1.000000000000000000, 0.000000000000000000, 0.000000000000000000 ) ) ;
#16544 = CARTESIAN_POINT ( 'NONE',  ( 0.000000000000000000, -5.000000000000000000, 9.068199145005368464E-15 ) ) ;
#16545 = ORIENTED_EDGE ( 'NONE', *, *, #5405, .T. ) ;
#16546 = AXIS2_PLACEMENT_3D ( 'NONE', #8660, #6837, #18987 ) ;
#16547 = VERTEX_POINT ( 'NONE', #127 ) ;
#16548 = ORIENTED_EDGE ( 'NONE', *, *, #6644, .T. ) ;
#16549 = EDGE_CURVE ( 'NONE', #384, #6508, #21794, .T. ) ;
#16550 = VERTEX_POINT ( 'NONE', #467 ) ;
#16551 = CYLINDRICAL_SURFACE ( 'NONE', #19493, 19.11328065563152379 ) ;
#16552 = DIRECTION ( 'NONE',  ( 0.000000000000000000, 1.000000000000000000, 0.000000000000000000 ) ) ;
#16553 = EDGE_LOOP ( 'NONE', ( #11622, #9901, #8861, #9908 ) ) ;
#16554 = CARTESIAN_POINT ( 'NONE',  ( -28.88846368933341324, -19.59430950039325836, -2.999999999999947153 ) ) ;
#16555 = CARTESIAN_POINT ( 'NONE',  ( -13.83143812983095344, 29.36548507648009831, 2.999999999999995559 ) ) ;
#16556 = EDGE_LOOP ( 'NONE', ( #10789, #6348, #10397, #2977 ) ) ;
#16557 = EDGE_CURVE ( 'NONE', #19747, #2560, #15904, .T. ) ;
#16558 = ORIENTED_EDGE ( 'NONE', *, *, #5324, .T. ) ;
#16559 = CARTESIAN_POINT ( 'NONE',  ( 3.330669073875469621E-13, -1.110223024625156540E-13, -2.999999999999971578 ) ) ;
#16560 = CARTESIAN_POINT ( 'NONE',  ( -9.952189117650803496, 40.00000000000000000, 53.64426396172073908 ) ) ;
#16561 = CARTESIAN_POINT ( 'NONE',  ( 35.00000000000001421, 4.000000000000028422, 1.540743955509788682E-30 ) ) ;
#16562 = CARTESIAN_POINT ( 'NONE',  ( 2.775557561562891351E-14, 2.775557561562891351E-14, 5.750000000000001776 ) ) ;
#16563 = AXIS2_PLACEMENT_3D ( 'NONE', #14652, #22116, #5956 ) ;
#16564 = AXIS2_PLACEMENT_3D ( 'NONE', #12766, #18162, #5789 ) ;
#16565 = CARTESIAN_POINT ( 'NONE',  ( -2.576224933359605451, 39.84426458497861745, 51.65025110504824113 ) ) ;
#16566 = EDGE_CURVE ( 'NONE', #7291, #11481, #243, .T. ) ;
#16567 = DIRECTION ( 'NONE',  ( -1.000000000000000000, 1.301042606982605814E-16, 0.000000000000000000 ) ) ;
#16568 = ORIENTED_EDGE ( 'NONE', *, *, #7122, .T. ) ;
#16569 = ORIENTED_EDGE ( 'NONE', *, *, #12117, .T. ) ;
#16570 = ADVANCED_FACE ( 'NONE', ( #3477 ), #7123, .T. ) ;
#16571 = EDGE_LOOP ( 'NONE', ( #8658, #21185 ) ) ;
#16572 = CARTESIAN_POINT ( 'NONE',  ( -19.88905041090809434, 17.72428093568618479, 58.11830361000903622 ) ) ;
#16573 = FACE_OUTER_BOUND ( 'NONE', #16111, .T. ) ;
#16574 = CIRCLE ( 'NONE', #9263, 3.999999999999998224 ) ;
#16575 = B_SPLINE_CURVE_WITH_KNOTS ( 'NONE', 3,
 ( #8635, #22640, #12846, #5528 ),
 .UNSPECIFIED., .F., .F.,
 ( 4, 4 ),
 ( 0.001893031756885543487, 0.003808480026563717744 ),
 .UNSPECIFIED. ) ;
#16576 = DIRECTION ( 'NONE',  ( -1.000000000000000000, 0.000000000000000000, 0.000000000000000000 ) ) ;
#16577 = AXIS2_PLACEMENT_3D ( 'NONE', #12172, #10552, #13761 ) ;
#16578 = DIRECTION ( 'NONE',  ( -6.505213034913038160E-19, -3.903127820947822896E-18, -1.000000000000000000 ) ) ;
#16579 = DIRECTION ( 'NONE',  ( 0.000000000000000000, -1.000000000000000000, 0.000000000000000000 ) ) ;
#16580 = CARTESIAN_POINT ( 'NONE',  ( -5.905663676014976105, 39.12131202908561534, -53.51378431580162953 ) ) ;
#16581 = LINE ( 'NONE', #888, #5348 ) ;
#16582 = FACE_OUTER_BOUND ( 'NONE', #11205, .T. ) ;
#16583 = EDGE_LOOP ( 'NONE', ( #22520, #6130, #979, #283 ) ) ;
#16584 = DIRECTION ( 'NONE',  ( -0.000000000000000000, 1.000000000000000000, -0.000000000000000000 ) ) ;
#16585 = CARTESIAN_POINT ( 'NONE',  ( 42.50000000000000711, -5.000000000000000000, 47.50000000000000711 ) ) ;
#16586 = DIRECTION ( 'NONE',  ( 6.505213034913038160E-19, 3.903127820947822896E-18, 1.000000000000000000 ) ) ;
#16587 = CARTESIAN_POINT ( 'NONE',  ( -90.00000000000000000, 40.00000000000000711, 2.524999999999998579 ) ) ;
#16588 = ORIENTED_EDGE ( 'NONE', *, *, #18287, .F. ) ;
#16589 = PLANE ( 'NONE',  #21164 ) ;
#16590 = AXIS2_PLACEMENT_3D ( 'NONE', #16478, #1124, #8118 ) ;
#16591 = ORIENTED_EDGE ( 'NONE', *, *, #6767, .F. ) ;
#16592 = EDGE_CURVE ( 'NONE', #5838, #15378, #8619, .T. ) ;
#16593 = CYLINDRICAL_SURFACE ( 'NONE', #12252, 0.9999999999999995559 ) ;
#16594 = DIRECTION ( 'NONE',  ( -1.000000000000000000, 1.530638361156006492E-16, 0.000000000000000000 ) ) ;
#16595 = AXIS2_PLACEMENT_3D ( 'NONE', #20969, #10293, #20515 ) ;
#16596 = AXIS2_PLACEMENT_3D ( 'NONE', #13848, #10188, #1495 ) ;
#16597 = EDGE_CURVE ( 'NONE', #9062, #17126, #10894, .T. ) ;
#16598 = EDGE_CURVE ( 'NONE', #104, #384, #3869, .T. ) ;
#16599 = EDGE_LOOP ( 'NONE', ( #9550, #9237 ) ) ;
#16600 = EDGE_CURVE ( 'NONE', #15903, #20662, #4965, .T. ) ;
#16601 = CARTESIAN_POINT ( 'NONE',  ( 31.21605069118085751, 8.646032897228927538, -6.999999999999950262 ) ) ;
#16602 = AXIS2_PLACEMENT_3D ( 'NONE', #17353, #14005, #19320 ) ;
#16603 = CARTESIAN_POINT ( 'NONE',  ( 42.50000000000000711, -12.00000000000012434, -47.50000000000000000 ) ) ;
#16604 = EDGE_LOOP ( 'NONE', ( #7721, #8430 ) ) ;
#16605 = CARTESIAN_POINT ( 'NONE',  ( 42.50000000000000711, -9.600000000000001421, -45.00000000000000000 ) ) ;
#16606 = DIRECTION ( 'NONE',  ( -1.000000000000000000, -9.076011110974242363E-16, 0.000000000000000000 ) ) ;
#16607 = VECTOR ( 'NONE', #7188, 1000.000000000000000 ) ;
#16608 = EDGE_CURVE ( 'NONE', #2332, #11150, #21067, .T. ) ;
#16609 = DIRECTION ( 'NONE',  ( 1.000000000000000000, 0.000000000000000000, 0.000000000000000000 ) ) ;
#16610 = CARTESIAN_POINT ( 'NONE',  ( -34.99999999999980815, 40.00000000000000000, 57.09999999999921982 ) ) ;
#16611 = CARTESIAN_POINT ( 'NONE',  ( -16.37028666998709880, 4.520534895874758874, -57.04777702420076935 ) ) ;
#16612 = AXIS2_PLACEMENT_3D ( 'NONE', #7795, #13046, #6304 ) ;
#16613 = CARTESIAN_POINT ( 'NONE',  ( -0.7796821504949128512, 40.00000000000002132, 49.24007756836347482 ) ) ;
#16614 = DIRECTION ( 'NONE',  ( -0.4332438415859285463, 0.000000000000000000, -0.9012767464701765263 ) ) ;
#16615 = ORIENTED_EDGE ( 'NONE', *, *, #15331, .F. ) ;
#16616 = DIRECTION ( 'NONE',  ( -1.000000000000000000, -1.208970125616044077E-17, 0.000000000000000000 ) ) ;
#16617 = FACE_OUTER_BOUND ( 'NONE', #3511, .T. ) ;
#16618 = CARTESIAN_POINT ( 'NONE',  ( -42.50000000000000711, -5.000000000000000000, 47.50000000000000711 ) ) ;
#16619 = EDGE_LOOP ( 'NONE', ( #2258, #3544, #8298 ) ) ;
#16620 =( REPRESENTATION_RELATIONSHIP ('NONE','NONE', #8442, #10907 ) REPRESENTATION_RELATIONSHIP_WITH_TRANSFORMATION ( #21197 )SHAPE_REPRESENTATION_RELATIONSHIP( ) );
#16621 = CIRCLE ( 'NONE', #884, 2.500000000000002220 ) ;
#16622 = CARTESIAN_POINT ( 'NONE',  ( -14.40375226887235982, 24.20453657423044902, 45.56106839101557426 ) ) ;
#16623 = CARTESIAN_POINT ( 'NONE',  ( 27.19760187735870005, 24.73600648735113694, -1.999999999999977573 ) ) ;
#16624 = PRODUCT_DEFINITION_SHAPE ( 'NONE', 'NONE',  #22701 ) ;
#16625 = VECTOR ( 'NONE', #15062, 1000.000000000000000 ) ;
#16626 = AXIS2_PLACEMENT_3D ( 'NONE', #14462, #21474, #19870 ) ;
#16627 = VERTEX_POINT ( 'NONE', #7351 ) ;
#16628 = VERTEX_POINT ( 'NONE', #19287 ) ;
#16629 = DIRECTION ( 'NONE',  ( 0.9896250438806505345, -0.1436365362847020488, 0.003289068006899746859 ) ) ;
#16630 = ADVANCED_FACE ( 'NONE', ( #3593 ), #5411, .T. ) ;
#16631 = ORIENTED_EDGE ( 'NONE', *, *, #10596, .F. ) ;
#16632 = FACE_OUTER_BOUND ( 'NONE', #4575, .T. ) ;
#16633 = DIRECTION ( 'NONE',  ( 0.000000000000000000, 0.000000000000000000, 1.000000000000000000 ) ) ;
#16634 = CARTESIAN_POINT ( 'NONE',  ( 2.602085213965210642E-15, -0.9047447100419790944, 0.000000000000000000 ) ) ;
#16635 = ADVANCED_FACE ( 'NONE', ( #19952 ), #14434, .T. ) ;
#16636 = FACE_OUTER_BOUND ( 'NONE', #4947, .T. ) ;
#16637 = CARTESIAN_POINT ( 'NONE',  ( 4.076028284553002479, 5.556537143872661844, -39.58813741008490439 ) ) ;
#16638 = VERTEX_POINT ( 'NONE', #7922 ) ;
#16639 = DIRECTION ( 'NONE',  ( -1.000000000000000000, 0.000000000000000000, 0.000000000000000000 ) ) ;
#16640 = CARTESIAN_POINT ( 'NONE',  ( -42.50000000000000711, -9.600000000000001421, -45.00000000000000000 ) ) ;
#16641 = ORIENTED_EDGE ( 'NONE', *, *, #12295, .F. ) ;
#16642 = CARTESIAN_POINT ( 'NONE',  ( 5.833333333333329485, 0.000000000000000000, -40.61164310337066041 ) ) ;
#16643 = AXIS2_PLACEMENT_3D ( 'NONE', #13362, #4689, #11668 ) ;
#16644 = CARTESIAN_POINT ( 'NONE',  ( 19.60425726290408122, 16.02072691545760463, -60.52684394361300235 ) ) ;
#16645 = EDGE_LOOP ( 'NONE', ( #12917, #1473, #16491, #10358 ) ) ;
#16646 = CARTESIAN_POINT ( 'NONE',  ( -1.570150081433425937, 40.00000000000000000, -49.72616478525270622 ) ) ;
#16647 = CARTESIAN_POINT ( 'NONE',  ( 0.6233897118003356441, 39.99089506582289744, -49.47139888151590270 ) ) ;
#16648 = EDGE_CURVE ( 'NONE', #6745, #8848, #567, .T. ) ;
#16649 = EDGE_LOOP ( 'NONE', ( #9780, #2231, #799 ) ) ;
#16650 = DIRECTION ( 'NONE',  ( -1.000000000000000000, -1.208970125616063644E-17, 0.000000000000000000 ) ) ;
#16651 = CARTESIAN_POINT ( 'NONE',  ( -34.99999999999997868, 0.000000000000000000, 57.49999999999699440 ) ) ;
#16652 = VERTEX_POINT ( 'NONE', #11234 ) ;
#16653 = CARTESIAN_POINT ( 'NONE',  ( 10.79594548525664699, 39.62239930148019340, 54.90840750699845074 ) ) ;
#16654 = LINE ( 'NONE', #4754, #21337 ) ;
#16655 = AXIS2_PLACEMENT_3D ( 'NONE', #6943, #18417, #13355 ) ;
#16656 = VECTOR ( 'NONE', #10059, 1000.000000000000000 ) ;
#16657 = CARTESIAN_POINT ( 'NONE',  ( 22.40268525210799311, 21.30540434957255513, -58.66274428449842304 ) ) ;
#16658 = ORIENTED_EDGE ( 'NONE', *, *, #7537, .F. ) ;
#16659 = CIRCLE ( 'NONE', #3120, 36.76383501243555685 ) ;
#16660 = EDGE_CURVE ( 'NONE', #5679, #1150, #16669, .T. ) ;
#16661 = ORIENTED_EDGE ( 'NONE', *, *, #20797, .F. ) ;
#16662 = VERTEX_POINT ( 'NONE', #21443 ) ;
#16663 = ORIENTED_EDGE ( 'NONE', *, *, #2954, .T. ) ;
#16664 = DIRECTION ( 'NONE',  ( 0.000000000000000000, 0.000000000000000000, -1.000000000000000000 ) ) ;
#16665 = EDGE_LOOP ( 'NONE', ( #6313, #10902, #17472, #9565 ) ) ;
#16666 = CARTESIAN_POINT ( 'NONE',  ( -90.00000000000000000, 39.97500000000000142, -9.108981535246192915E-16 ) ) ;
#16667 = CARTESIAN_POINT ( 'NONE',  ( 35.00000000000000000, 40.00000000000000000, -58.99999999999993605 ) ) ;
#16668 = VERTEX_POINT ( 'NONE', #18231 ) ;
#16669 = CIRCLE ( 'NONE', #6794, 2.499999999999998668 ) ;
#16670 = DIRECTION ( 'NONE',  ( 6.505213034913038160E-19, 3.903127820947822896E-18, 1.000000000000000000 ) ) ;
#16671 = AXIS2_PLACEMENT_3D ( 'NONE', #4201, #7978, #11172 ) ;
#16672 = ORIENTED_EDGE ( 'NONE', *, *, #5558, .F. ) ;
#16673 = LINE ( 'NONE', #2708, #13372 ) ;
#16674 = CIRCLE ( 'NONE', #21432, 36.76383501243555685 ) ;
#16675 = DIRECTION ( 'NONE',  ( 0.000000000000000000, 0.000000000000000000, 1.000000000000000000 ) ) ;
#16676 = DIRECTION ( 'NONE',  ( 0.000000000000000000, 0.000000000000000000, 1.000000000000000000 ) ) ;
#16677 = CARTESIAN_POINT ( 'NONE',  ( -35.29097153256766006, -4.153395668489732628, -2.999999999999994671 ) ) ;
#16678 = EDGE_CURVE ( 'NONE', #6038, #22156, #19593, .T. ) ;
#16679 = CARTESIAN_POINT ( 'NONE',  ( -7.017626609043913000, 6.725442770851620899, 41.44244536674935375 ) ) ;
#16680 = DIRECTION ( 'NONE',  ( -1.000000000000000000, 0.000000000000000000, 0.000000000000000000 ) ) ;
#16681 = CIRCLE ( 'NONE', #13728, 2.500000000000002220 ) ;
#16682 = CIRCLE ( 'NONE', #11564, 0.9999999999999995559 ) ;
#16683 = ORIENTED_EDGE ( 'NONE', *, *, #10655, .T. ) ;
#16684 = EDGE_CURVE ( 'NONE', #10389, #19954, #20880, .T. ) ;
#16685 = CIRCLE ( 'NONE', #12304, 41.00000000000000000 ) ;
#16686 = ADVANCED_FACE ( 'NONE', ( #21672 ), #5969, .T. ) ;
#16687 = VERTEX_POINT ( 'NONE', #11466 ) ;
#16688 = VERTEX_POINT ( 'NONE', #18454 ) ;
#16689 = CARTESIAN_POINT ( 'NONE',  ( -19.23518390577171999, 25.54875756131827558, 60.43569366689264655 ) ) ;
#16690 = AXIS2_PLACEMENT_3D ( 'NONE', #14859, #16831, #14973 ) ;
#16691 = CARTESIAN_POINT ( 'NONE',  ( -23.65408649739099545, -22.22891329980544839, -6.999999999999950262 ) ) ;
#16692 = CARTESIAN_POINT ( 'NONE',  ( 1.110223024625156540E-13, -5.551115123125782702E-14, -6.999999999999950262 ) ) ;
#16693 = CARTESIAN_POINT ( 'NONE',  ( 1.438414332626293479, -1.268869129819692798, -49.24051559643684328 ) ) ;
#16694 = FACE_BOUND ( 'NONE', #15837, .T. ) ;
#16695 = EDGE_CURVE ( 'NONE', #10325, #19599, #15189, .T. ) ;
#16696 = CARTESIAN_POINT ( 'NONE',  ( 34.99999999999980815, 40.00000000000000000, 54.99999999999922551 ) ) ;
#16697 = LINE ( 'NONE', #16353, #4998 ) ;
#16698 = CARTESIAN_POINT ( 'NONE',  ( 42.50000000000000711, -5.000000000000000000, -47.50000000000000000 ) ) ;
#16699 = AXIS2_PLACEMENT_3D ( 'NONE', #10884, #15806, #21319 ) ;
#16700 = CARTESIAN_POINT ( 'NONE',  ( -0.7060534721732323327, 40.00000000000297007, -49.41655051369872353 ) ) ;
#16701 = DIRECTION ( 'NONE',  ( 0.000000000000000000, 0.000000000000000000, -1.000000000000000000 ) ) ;
#16702 = AXIS2_PLACEMENT_3D ( 'NONE', #2764, #9746, #15220 ) ;
#16703 = ORIENTED_EDGE ( 'NONE', *, *, #22394, .F. ) ;
#16704 = DIRECTION ( 'NONE',  ( -1.000000000000000000, 0.000000000000000000, 0.000000000000000000 ) ) ;
#16705 = CARTESIAN_POINT ( 'NONE',  ( -89.99999999999701572, 0.000000000000000000, -3.012171160963566127E-14 ) ) ;
#16706 = DIRECTION ( 'NONE',  ( 0.000000000000000000, -1.000000000000000000, 0.000000000000000000 ) ) ;
#16707 = EDGE_CURVE ( 'NONE', #22419, #4210, #8851, .T. ) ;
#16708 = DIRECTION ( 'NONE',  ( -1.000000000000000000, -1.208970125616081209E-17, 0.000000000000000000 ) ) ;
#16709 = CIRCLE ( 'NONE', #3555, 19.99999999999999289 ) ;
#16710 = ORIENTED_EDGE ( 'NONE', *, *, #13287, .F. ) ;
#16711 = ORIENTED_EDGE ( 'NONE', *, *, #3309, .F. ) ;
#16712 = CARTESIAN_POINT ( 'NONE',  ( -4.084299015953638090, -4.682619376883241813, -48.27507093818995543 ) ) ;
#16713 = CARTESIAN_POINT ( 'NONE',  ( -12.31876324338271367, -30.07487443287973505, -2.999999999999995559 ) ) ;
#16714 = EDGE_CURVE ( 'NONE', #11218, #18097, #3340, .T. ) ;
#16715 = CIRCLE ( 'NONE', #13028, 0.9999999999999974465 ) ;
#16716 = CARTESIAN_POINT ( 'NONE',  ( -20.00000000000001421, 20.00000000000000000, -98.00000000000000000 ) ) ;
#16717 = DIRECTION ( 'NONE',  ( -0.000000000000000000, 1.000000000000000000, -0.000000000000000000 ) ) ;
#16718 = ORIENTED_EDGE ( 'NONE', *, *, #5407, .T. ) ;
#16719 = CARTESIAN_POINT ( 'NONE',  ( 1.952251977614869904, 39.97720309756248014, -50.19198521789787293 ) ) ;
#16720 = CARTESIAN_POINT ( 'NONE',  ( 10.72803533575908119, 39.99999999999999289, 53.87712872072329162 ) ) ;
#16721 = ADVANCED_FACE ( 'NONE', ( #6542 ), #16303, .T. ) ;
#16722 = CARTESIAN_POINT ( 'NONE',  ( -34.99999999999997868, -5.000000000000000000, 54.99999999999698730 ) ) ;
#16723 = CARTESIAN_POINT ( 'NONE',  ( -4.873423496009598566, 40.00000000000000000, 51.54632858871904233 ) ) ;
#16724 = CARTESIAN_POINT ( 'NONE',  ( 11.17438353485539615, 39.11312751370834206, -55.08132212994122767 ) ) ;
#16725 = CARTESIAN_POINT ( 'NONE',  ( -5.833333333333341919, 33.81926995981417150, -40.61164310337066041 ) ) ;
#16726 = CARTESIAN_POINT ( 'NONE',  ( -34.99999999999999289, -5.000000000000000000, -3.012171160963566127E-14 ) ) ;
#16727 = VERTEX_POINT ( 'NONE', #13501 ) ;
#16728 = FACE_OUTER_BOUND ( 'NONE', #12773, .T. ) ;
#16729 = CIRCLE ( 'NONE', #9784, 0.9999999999999974465 ) ;
#16730 = DIRECTION ( 'NONE',  ( -1.000000000000000000, -1.208970125616044077E-17, 0.000000000000000000 ) ) ;
#16731 = DIRECTION ( 'NONE',  ( -0.000000000000000000, -0.000000000000000000, 1.000000000000000000 ) ) ;
#16732 = DIRECTION ( 'NONE',  ( -6.505213034913038160E-19, -3.903127820947822896E-18, -1.000000000000000000 ) ) ;
#16733 = EDGE_CURVE ( 'NONE', #22498, #2692, #19983, .T. ) ;
#16734 = DIRECTION ( 'NONE',  ( -1.000000000000000000, 0.000000000000000000, 0.000000000000000000 ) ) ;
#16735 = AXIS2_PLACEMENT_3D ( 'NONE', #20279, #6064, #18552 ) ;
#16736 = ORIENTED_EDGE ( 'NONE', *, *, #4990, .F. ) ;
#16737 = CARTESIAN_POINT ( 'NONE',  ( 2.775557561562891351E-14, -2.775557561562891351E-14, 2.999999999999995559 ) ) ;
#16738 = VECTOR ( 'NONE', #15595, 1000.000000000000000 ) ;
#16739 = CIRCLE ( 'NONE', #5410, 41.00000000000000000 ) ;
#16740 = ORIENTED_EDGE ( 'NONE', *, *, #16043, .T. ) ;
#16741 = CONICAL_SURFACE ( 'NONE', #11614, 2.524999999999999467, 0.7853981633973095011 ) ;
#16742 = CIRCLE ( 'NONE', #17840, 2.000000000000001776 ) ;
#16743 = VERTEX_POINT ( 'NONE', #11693 ) ;
#16744 = ADVANCED_FACE ( 'NONE', ( #8037 ), #20519, .F. ) ;
#16745 = CARTESIAN_POINT ( 'NONE',  ( 153.3434499333752115, 176.6715123837293504, -11.64191406197529766 ) ) ;
#16746 = CIRCLE ( 'NONE', #1759, 19.11328065563151668 ) ;
#16747 = ORIENTED_EDGE ( 'NONE', *, *, #12254, .T. ) ;
#16748 = CARTESIAN_POINT ( 'NONE',  ( 19.85669122310594759, 22.43861522864551006, 60.58781117059878341 ) ) ;
#16749 = CARTESIAN_POINT ( 'NONE',  ( 10.49999999999994138, 42.51666049839543149, 100.0000000000000000 ) ) ;
#16750 = CARTESIAN_POINT ( 'NONE',  ( -30.00000000000001421, 20.00000000000000711, -105.0000000000000142 ) ) ;
#16751 = CARTESIAN_POINT ( 'NONE',  ( 35.00000000000000711, 39.00000000000000711, 49.99999999999999289 ) ) ;
#16752 = EDGE_CURVE ( 'NONE', #5200, #16771, #14088, .T. ) ;
#16753 = CARTESIAN_POINT ( 'NONE',  ( 1.054992083789042301, 5.028051073338380306, -38.77590480715000609 ) ) ;
#16754 = ORIENTED_EDGE ( 'NONE', *, *, #18064, .T. ) ;
#16755 = DIRECTION ( 'NONE',  ( -0.000000000000000000, 1.000000000000000000, -0.000000000000000000 ) ) ;
#16756 = CARTESIAN_POINT ( 'NONE',  ( -34.99999999999999289, -3.999999999999985345, 59.99999999999698019 ) ) ;
#16757 = ORIENTED_EDGE ( 'NONE', *, *, #17016, .F. ) ;
#16758 = CARTESIAN_POINT ( 'NONE',  ( -8.759110511859024228, 7.803016162472655282, -42.56552456877078328 ) ) ;
#16759 = DIRECTION ( 'NONE',  ( 0.000000000000000000, 0.000000000000000000, 1.000000000000000000 ) ) ;
#16760 = LINE ( 'NONE', #20541, #2400 ) ;
#16761 = DIRECTION ( 'NONE',  ( -6.505213034913038160E-19, -3.903127820947822896E-18, -1.000000000000000000 ) ) ;
#16762 = EDGE_LOOP ( 'NONE', ( #13891, #16286, #16186, #9812 ) ) ;
#16763 = CARTESIAN_POINT ( 'NONE',  ( 34.88850421923977763, -1.128083539116253586, 3.000000000000023537 ) ) ;
#16764 = CARTESIAN_POINT ( 'NONE',  ( 35.00000000000001421, -5.000000000000000000, 1.540743955509788682E-30 ) ) ;
#16765 = CIRCLE ( 'NONE', #3963, 9.000000000000035527 ) ;
#16766 = EDGE_LOOP ( 'NONE', ( #12808, #4780, #21476, #21494 ) ) ;
#16767 = DIRECTION ( 'NONE',  ( -6.505213034913038160E-19, -3.903127820947822896E-18, -1.000000000000000000 ) ) ;
#16768 = FACE_OUTER_BOUND ( 'NONE', #19633, .T. ) ;
#16769 = EDGE_CURVE ( 'NONE', #7646, #16668, #2430, .T. ) ;
#16770 = CONICAL_SURFACE ( 'NONE', #7261, 58.99999999999994316, 0.7853981633974725929 ) ;
#16771 = VERTEX_POINT ( 'NONE', #4932 ) ;
#16772 = UNCERTAINTY_MEASURE_WITH_UNIT (LENGTH_MEASURE( 1.000000000000000082E-05 ), #7360, 'distance_accuracy_value', 'NONE');
#16773 = CARTESIAN_POINT ( 'NONE',  ( 11.87139216507892847, 36.11857111619715255, 55.37976054165663697 ) ) ;
#16774 = DIRECTION ( 'NONE',  ( -0.000000000000000000, -1.000000000000000000, -0.000000000000000000 ) ) ;
#16775 = AXIS2_PLACEMENT_3D ( 'NONE', #3056, #18525, #10030 ) ;
#16776 = EDGE_CURVE ( 'NONE', #11978, #15147, #3152, .T. ) ;
#16777 = EDGE_CURVE ( 'NONE', #2480, #17245, #3221, .T. ) ;
#16778 = CARTESIAN_POINT ( 'NONE',  ( 20.01704759191777683, 20.30656121191836405, -60.62580324356297012 ) ) ;
#16779 = ORIENTED_EDGE ( 'NONE', *, *, #4506, .T. ) ;
#16780 = ORIENTED_EDGE ( 'NONE', *, *, #10469, .F. ) ;
#16781 = CIRCLE ( 'NONE', #1044, 31.50000000000000000 ) ;
#16782 = EDGE_CURVE ( 'NONE', #19286, #20094, #14476, .T. ) ;
#16783 = EDGE_LOOP ( 'NONE', ( #1920, #15376, #2348, #18607 ) ) ;
#16784 = ORIENTED_EDGE ( 'NONE', *, *, #2201, .F. ) ;
#16785 = CARTESIAN_POINT ( 'NONE',  ( 11.69583326050833172, 39.02781355202390756, 55.28967510510689465 ) ) ;
#16786 = AXIS2_PLACEMENT_3D ( 'NONE', #14133, #14016, #3519 ) ;
#16787 = TOROIDAL_SURFACE ( 'NONE', #9096, 22.00000000000000000, 2.000000000000000000 ) ;
#16788 = ORIENTED_EDGE ( 'NONE', *, *, #17800, .T. ) ;
#16789 = DIRECTION ( 'NONE',  ( 1.000000000000000000, 0.000000000000000000, 0.000000000000000000 ) ) ;
#16790 = DIRECTION ( 'NONE',  ( -0.000000000000000000, 1.000000000000000000, -0.000000000000000000 ) ) ;
#16791 = EDGE_LOOP ( 'NONE', ( #18980, #21261, #11290, #8901, #19414, #12039 ) ) ;
#16792 = CIRCLE ( 'NONE', #8013, 2.500000000000008882 ) ;
#16793 = DIRECTION ( 'NONE',  ( -0.000000000000000000, 1.000000000000000000, -0.000000000000000000 ) ) ;
#16794 = VERTEX_POINT ( 'NONE', #13390 ) ;
#16795 = DIRECTION ( 'NONE',  ( -1.000000000000000000, -1.208970125616063644E-17, 0.000000000000000000 ) ) ;
#16796 = DIRECTION ( 'NONE',  ( -0.000000000000000000, -1.000000000000000000, -0.000000000000000000 ) ) ;
#16797 = CARTESIAN_POINT ( 'NONE',  ( -42.50000000000000711, -9.600000000000001421, -47.50000000000000000 ) ) ;
#16798 = CARTESIAN_POINT ( 'NONE',  ( -0.2573524306472053103, 39.99960945630349585, 48.93325698110795230 ) ) ;
#16799 = CIRCLE ( 'NONE', #6544, 2.500000000000002220 ) ;
#16800 = ADVANCED_FACE ( 'NONE', ( #9864 ), #5054, .F. ) ;
#16801 = DIRECTION ( 'NONE',  ( 1.000000000000000000, -1.084202172485504681E-16, 0.000000000000000000 ) ) ;
#16802 = CARTESIAN_POINT ( 'NONE',  ( -3.469446951953614189E-14, -5.000000000000000000, 48.73397172404114031 ) ) ;
#16803 = VERTEX_POINT ( 'NONE', #22128 ) ;
#16804 = VERTEX_POINT ( 'NONE', #2381 ) ;
#16805 = EDGE_CURVE ( 'NONE', #8029, #1297, #19908, .T. ) ;
#16806 = ORIENTED_EDGE ( 'NONE', *, *, #13890, .T. ) ;
#16807 = CARTESIAN_POINT ( 'NONE',  ( -18.09042992579668052, 28.57522027848806800, 57.61279183055282971 ) ) ;
#16808 = CARTESIAN_POINT ( 'NONE',  ( -30.00000000000001421, 20.00000000000000355, 100.0000000000000000 ) ) ;
#16809 = VECTOR ( 'NONE', #95, 1000.000000000000000 ) ;
#16810 = CYLINDRICAL_SURFACE ( 'NONE', #18222, 1.000000000000000888 ) ;
#16811 = CYLINDRICAL_SURFACE ( 'NONE', #7735, 59.99999999999700862 ) ;
#16812 = EDGE_CURVE ( 'NONE', #14951, #20662, #5565, .T. ) ;
#16813 = LINE ( 'NONE', #13461, #21818 ) ;
#16814 = ORIENTED_EDGE ( 'NONE', *, *, #8927, .F. ) ;
#16815 = DIRECTION ( 'NONE',  ( -0.000000000000000000, -1.000000000000000000, -0.000000000000000000 ) ) ;
#16816 = CARTESIAN_POINT ( 'NONE',  ( 2.220446049250313081E-13, -2.498001805406602216E-13, -6.859353255829918616 ) ) ;
#16817 = CARTESIAN_POINT ( 'NONE',  ( -6.803227178531130903, 38.81166136533656896, -55.43135129401765226 ) ) ;
#16818 = CARTESIAN_POINT ( 'NONE',  ( 35.00000000000058265, 28.00000000000000000, -55.00000000000076028 ) ) ;
#16819 = FACE_OUTER_BOUND ( 'NONE', #21133, .T. ) ;
#16820 = ADVANCED_FACE ( 'NONE', ( #19573 ), #18879, .F. ) ;
#16821 = PRODUCT_DEFINITION_SHAPE ( 'NONE', 'NONE',  #10506 ) ;
#16822 = ORIENTED_EDGE ( 'NONE', *, *, #7049, .T. ) ;
#16823 = DIRECTION ( 'NONE',  ( 0.000000000000000000, -1.000000000000000000, 0.000000000000000000 ) ) ;
#16824 = CARTESIAN_POINT ( 'NONE',  ( -10.48823472894017073, 39.21814192245744124, 54.82890001996310048 ) ) ;
#16825 = CARTESIAN_POINT ( 'NONE',  ( 42.50000000000000711, -5.000000000000000000, -54.00000000000000000 ) ) ;
#16826 = B_SPLINE_CURVE_WITH_KNOTS ( 'NONE', 3,
 ( #3819, #17788, #2093, #7476 ),
 .UNSPECIFIED., .F., .F.,
 ( 4, 4 ),
 ( 9.715086409102729949E-07, 0.001929643240672379145 ),
 .UNSPECIFIED. ) ;
#16827 = VERTEX_POINT ( 'NONE', #21291 ) ;
#16828 = CARTESIAN_POINT ( 'NONE',  ( 24.41514043009221524, 26.50842683089738117, 2.999999999999995559 ) ) ;
#16829 = AXIS2_PLACEMENT_3D ( 'NONE', #5243, #19108, #3533 ) ;
#16830 = DIRECTION ( 'NONE',  ( 0.000000000000000000, 0.000000000000000000, -1.000000000000000000 ) ) ;
#16831 = DIRECTION ( 'NONE',  ( -0.000000000000000000, 1.000000000000000000, -0.000000000000000000 ) ) ;
#16832 = ORIENTED_EDGE ( 'NONE', *, *, #15105, .F. ) ;
#16833 = ORIENTED_EDGE ( 'NONE', *, *, #13244, .T. ) ;
#16834 = CARTESIAN_POINT ( 'NONE',  ( -0.6808133077283172740, -3.155657370482437329, 47.81204852682553508 ) ) ;
#16835 = AXIS2_PLACEMENT_3D ( 'NONE', #22257, #12044, #13738 ) ;
#16836 = DIRECTION ( 'NONE',  ( -1.000000000000000000, 0.000000000000000000, 0.000000000000000000 ) ) ;
#16837 = ADVANCED_FACE ( 'NONE', ( #10968 ), #8990, .F. ) ;
#16838 = VERTEX_POINT ( 'NONE', #4675 ) ;
#16839 = FACE_OUTER_BOUND ( 'NONE', #6562, .T. ) ;
#16840 = AXIS2_PLACEMENT_3D ( 'NONE', #14447, #21579, #5761 ) ;
#16841 = FACE_OUTER_BOUND ( 'NONE', #2003, .T. ) ;
#16842 = CARTESIAN_POINT ( 'NONE',  ( -1.582598045080424232, 40.00000000000000000, 49.73344078919016198 ) ) ;
#16843 = CARTESIAN_POINT ( 'NONE',  ( 10.35284963817699300, 39.23826485918397822, -54.78050591800258218 ) ) ;
#16844 = DIRECTION ( 'NONE',  ( 6.505213034913038160E-19, 3.903127820947822896E-18, 1.000000000000000000 ) ) ;
#16845 = ADVANCED_FACE ( 'NONE', ( #8109 ), #2956, .F. ) ;
#16846 = LINE ( 'NONE', #20063, #17258 ) ;
#16847 = EDGE_LOOP ( 'NONE', ( #15982, #13500, #16494, #734 ) ) ;
#16848 = DIRECTION ( 'NONE',  ( 0.000000000000000000, 0.000000000000000000, -1.000000000000000000 ) ) ;
#16849 = LINE ( 'NONE', #13163, #876 ) ;
#16850 = CARTESIAN_POINT ( 'NONE',  ( -34.00000000000000000, -8.251288694035729065, 0.000000000000000000 ) ) ;
#16851 = DIRECTION ( 'NONE',  ( 0.000000000000000000, -1.000000000000000000, 0.000000000000000000 ) ) ;
#16852 = ORIENTED_EDGE ( 'NONE', *, *, #1553, .F. ) ;
#16853 = CIRCLE ( 'NONE', #6977, 36.76383501243555685 ) ;
#16854 = DIRECTION ( 'NONE',  ( 1.000000000000000000, 0.000000000000000000, 0.000000000000000000 ) ) ;
#16855 = LINE ( 'NONE', #19953, #3444 ) ;
#16856 = ADVANCED_FACE ( 'NONE', ( #1219 ), #15178, .T. ) ;
#16857 = ORIENTED_EDGE ( 'NONE', *, *, #4516, .T. ) ;
#16858 = ORIENTED_EDGE ( 'NONE', *, *, #4758, .T. ) ;
#16859 = EDGE_CURVE ( 'NONE', #5003, #21713, #16813, .T. ) ;
#16860 = EDGE_LOOP ( 'NONE', ( #5523, #2972, #17502, #6202 ) ) ;
#16861 = CARTESIAN_POINT ( 'NONE',  ( 14.32898074910538710, 33.98521869245691107, 58.94425321795622352 ) ) ;
#16862 = DIRECTION ( 'NONE',  ( 6.505213034913038160E-19, 3.903127820947822896E-18, 1.000000000000000000 ) ) ;
#16863 = AXIS2_PLACEMENT_3D ( 'NONE', #9537, #2669, #824 ) ;
#16864 = DIRECTION ( 'NONE',  ( -0.000000000000000000, -0.000000000000000000, 1.000000000000000000 ) ) ;
#16865 = CARTESIAN_POINT ( 'NONE',  ( 16.97759837164270280, 9.398593820328089876, 59.81443117571823365 ) ) ;
#16866 = CARTESIAN_POINT ( 'NONE',  ( -5.833333333333337478, 6.180730040185833829, -40.61164310337066041 ) ) ;
#16867 = VERTEX_POINT ( 'NONE', #20370 ) ;
#16868 = DIRECTION ( 'NONE',  ( 0.000000000000000000, 1.000000000000000000, -0.000000000000000000 ) ) ;
#16869 = FACE_OUTER_BOUND ( 'NONE', #7769, .T. ) ;
#16870 = ORIENTED_EDGE ( 'NONE', *, *, #1179, .F. ) ;
#16871 = DIRECTION ( 'NONE',  ( -0.000000000000000000, -1.000000000000000000, -0.000000000000000000 ) ) ;
#16872 = CARTESIAN_POINT ( 'NONE',  ( 3.656418565264413445, 37.07861450834795392, -2.999999999999988898 ) ) ;
#16873 = LINE ( 'NONE', #4846, #1283 ) ;
#16874 = DIRECTION ( 'NONE',  ( -0.000000000000000000, 1.000000000000000000, -0.000000000000000000 ) ) ;
#16875 = ORIENTED_EDGE ( 'NONE', *, *, #14724, .F. ) ;
#16876 = CARTESIAN_POINT ( 'NONE',  ( -2.080482199426275746E-16, 39.99999999999997158, -48.73397172404480671 ) ) ;
#16877 = CARTESIAN_POINT ( 'NONE',  ( 4.240361389880744625, 39.54844917561619866, -53.29842195655537296 ) ) ;
#16878 = VERTEX_POINT ( 'NONE', #14958 ) ;
#16879 = FACE_OUTER_BOUND ( 'NONE', #15948, .T. ) ;
#16880 = CARTESIAN_POINT ( 'NONE',  ( 0.3444338182180646801, -0.009360450408019541091, -50.24963102686507455 ) ) ;
#16881 = ORIENTED_EDGE ( 'NONE', *, *, #7298, .T. ) ;
#16882 = DIRECTION ( 'NONE',  ( 1.445602896647339163E-16, 0.000000000000000000, 1.000000000000000000 ) ) ;
#16883 = DIRECTION ( 'NONE',  ( 0.000000000000000000, 0.000000000000000000, -1.000000000000000000 ) ) ;
#16884 = DIRECTION ( 'NONE',  ( -1.000000000000000000, -0.000000000000000000, -0.000000000000000000 ) ) ;
#16885 = CARTESIAN_POINT ( 'NONE',  ( 19.35294509712666766, 31.41613210955675228, -57.92571537617268973 ) ) ;
#16886 = EDGE_CURVE ( 'NONE', #4414, #18864, #2040, .T. ) ;
#16887 = ORIENTED_EDGE ( 'NONE', *, *, #13470, .F. ) ;
#16888 = EDGE_LOOP ( 'NONE', ( #12323, #20826, #16061, #12748 ) ) ;
#16889 = ADVANCED_FACE ( 'NONE', ( #9823 ), #18514, .F. ) ;
#16890 = ADVANCED_FACE ( 'NONE', ( #22204 ), #13345, .F. ) ;
#16891 = VERTEX_POINT ( 'NONE', #11649 ) ;
#16892 = CARTESIAN_POINT ( 'NONE',  ( 1.516119572518645597, 24.61474968626487581, 6.878942250887983612 ) ) ;
#16893 = LINE ( 'NONE', #1091, #13642 ) ;
#16894 = EDGE_LOOP ( 'NONE', ( #14979, #4416, #13200, #21006 ) ) ;
#16895 = CARTESIAN_POINT ( 'NONE',  ( -30.13956425491234725, -21.05198877411829272, -2.800654218530471251 ) ) ;
#16896 = CARTESIAN_POINT ( 'NONE',  ( -3.309563215937974423, -3.140776953258733517, -49.61090469809253278 ) ) ;
#16897 = ORIENTED_EDGE ( 'NONE', *, *, #7341, .F. ) ;
#16898 = CARTESIAN_POINT ( 'NONE',  ( -2.670518050928090137, 14.42800760928497539, 6.613211112165401140 ) ) ;
#16899 = ADVANCED_FACE ( 'NONE', ( #9706 ), #20481, .T. ) ;
#16900 = VERTEX_POINT ( 'NONE', #7998 ) ;
#16901 = FACE_OUTER_BOUND ( 'NONE', #8562, .T. ) ;
#16902 = EDGE_CURVE ( 'NONE', #1054, #22660, #22325, .T. ) ;
#16903 = CARTESIAN_POINT ( 'NONE',  ( -35.00000000000058265, 39.97500000000000142, -55.00000000000076028 ) ) ;
#16904 = CARTESIAN_POINT ( 'NONE',  ( 17.32050807568884210, -25.00000000000000000, -9.999999999999880984 ) ) ;
#16905 = CARTESIAN_POINT ( 'NONE',  ( -5.393609312304999323E-15, 7.957073895306289835, 0.000000000000000000 ) ) ;
#16906 = CIRCLE ( 'NONE', #7026, 2.499999999999998668 ) ;
#16907 = DIRECTION ( 'NONE',  ( 0.000000000000000000, 0.000000000000000000, -1.000000000000000000 ) ) ;
#16908 = ORIENTED_EDGE ( 'NONE', *, *, #20055, .T. ) ;
#16909 = VERTEX_POINT ( 'NONE', #2617 ) ;
#16910 = B_SPLINE_CURVE_WITH_KNOTS ( 'NONE', 3,
 ( #5797, #12770, #19783, #4086, #11054, #18043, #16331, #9348, #2814, #10009 ),
 .UNSPECIFIED., .F., .F.,
 ( 4, 2, 2, 2, 4 ),
 ( 5.485454109350892508E-19, 0.002975785561748033829, 0.005951571123496067657, 0.008927356685244100185, 0.01190314224699213705 ),
 .UNSPECIFIED. ) ;
#16911 = ORIENTED_EDGE ( 'NONE', *, *, #17328, .T. ) ;
#16912 = CARTESIAN_POINT ( 'NONE',  ( -19.98510692294888713, 21.15566478733060762, 58.14357129518347733 ) ) ;
#16913 = CARTESIAN_POINT ( 'NONE',  ( 12.99999999999993960, 42.51666049839543149, -100.0000000000000000 ) ) ;
#16914 = LINE ( 'NONE', #8214, #5064 ) ;
#16915 = DIRECTION ( 'NONE',  ( 1.000000000000000000, 0.000000000000000000, 0.000000000000000000 ) ) ;
#16916 = EDGE_CURVE ( 'NONE', #14700, #16628, #9728, .T. ) ;
#16917 = APPLICATION_CONTEXT ( 'automotive_design' ) ;
#16918 = AXIS2_PLACEMENT_3D ( 'NONE', #9221, #10816, #510 ) ;
#16919 = ADVANCED_FACE ( 'NONE', ( #16694, #4560 ), #11539, .F. ) ;
#16920 = VERTEX_POINT ( 'NONE', #21129 ) ;
#16921 = CARTESIAN_POINT ( 'NONE',  ( 25.00000000000000000, 20.00000000000000000, 6.487780019669002523E-15 ) ) ;
#16922 = FACE_OUTER_BOUND ( 'NONE', #521, .T. ) ;
#16923 = DIRECTION ( 'NONE',  ( 0.000000000000000000, -1.000000000000000000, 0.000000000000000000 ) ) ;
#16924 = DIRECTION ( 'NONE',  ( -0.000000000000000000, 1.000000000000000000, -0.000000000000000000 ) ) ;
#16925 = ORIENTED_EDGE ( 'NONE', *, *, #10715, .F. ) ;
#16926 = EDGE_CURVE ( 'NONE', #10638, #11390, #8970, .T. ) ;
#16927 = FACE_OUTER_BOUND ( 'NONE', #10761, .T. ) ;
#16928 = DIRECTION ( 'NONE',  ( -6.505213034913038160E-19, -3.903127820947822896E-18, -1.000000000000000000 ) ) ;
#16929 = ORIENTED_EDGE ( 'NONE', *, *, #22522, .F. ) ;
#16930 = CARTESIAN_POINT ( 'NONE',  ( 2.775557561562891351E-14, -2.775557561562891351E-14, 2.999999999999999112 ) ) ;
#16931 = DIRECTION ( 'NONE',  ( 0.000000000000000000, 1.000000000000000000, 0.000000000000000000 ) ) ;
#16932 = CARTESIAN_POINT ( 'NONE',  ( 35.00000000000000000, 22.00000000000000711, 2.255140518769849223E-14 ) ) ;
#16933 = ORIENTED_EDGE ( 'NONE', *, *, #5165, .T. ) ;
#16934 = CIRCLE ( 'NONE', #822, 1.000000000000000888 ) ;
#16935 = AXIS2_PLACEMENT_3D ( 'NONE', #16986, #20553, #4410 ) ;
#16936 = ORIENTED_EDGE ( 'NONE', *, *, #3680, .F. ) ;
#16937 = CARTESIAN_POINT ( 'NONE',  ( -35.00000000000000000, 17.00000000000000000, -38.99999999999999289 ) ) ;
#16938 = ADVANCED_FACE ( 'NONE', ( #7484 ), #1879, .F. ) ;
#16939 = DIRECTION ( 'NONE',  ( 0.000000000000000000, 0.000000000000000000, -1.000000000000000000 ) ) ;
#16940 = ORIENTED_EDGE ( 'NONE', *, *, #12604, .T. ) ;
#16941 = DIRECTION ( 'NONE',  ( 1.000000000000000000, 1.208970125616053475E-17, 0.000000000000000000 ) ) ;
#16942 = CARTESIAN_POINT ( 'NONE',  ( -1.054992083788969470, 34.97194892666163213, -38.77590480714997767 ) ) ;
#16943 = FACE_OUTER_BOUND ( 'NONE', #10184, .T. ) ;
#16944 = CARTESIAN_POINT ( 'NONE',  ( -17.83677152930542675, 10.91058841726865403, -60.06362461869091618 ) ) ;
#16945 = LINE ( 'NONE', #4593, #1536 ) ;
#16946 = ORIENTED_EDGE ( 'NONE', *, *, #16733, .F. ) ;
#16947 = CARTESIAN_POINT ( 'NONE',  ( 14.17374118098243763, 24.92453540474833673, 45.45638825402599537 ) ) ;
#16948 = FACE_OUTER_BOUND ( 'NONE', #21462, .T. ) ;
#16949 = CARTESIAN_POINT ( 'NONE',  ( 37.07861450834818129, -3.656418565264246467, 3.000000000000023537 ) ) ;
#16950 = CARTESIAN_POINT ( 'NONE',  ( 23.65408649739122993, 22.22891329980541997, -2.999999999999971578 ) ) ;
#16951 = VECTOR ( 'NONE', #6238, 1000.000000000000000 ) ;
#16952 = EDGE_LOOP ( 'NONE', ( #115, #8388, #12708, #6734 ) ) ;
#16953 = LINE ( 'NONE', #11235, #16225 ) ;
#16954 = FACE_OUTER_BOUND ( 'NONE', #47, .T. ) ;
#16955 = ADVANCED_FACE ( 'NONE', ( #7141 ), #8862, .T. ) ;
#16956 = AXIS2_PLACEMENT_3D ( 'NONE', #10585, #12199, #12419 ) ;
#16957 = ORIENTED_EDGE ( 'NONE', *, *, #10802, .F. ) ;
#16958 = AXIS2_PLACEMENT_3D ( 'NONE', #402, #2354, #16093 ) ;
#16959 = ORIENTED_EDGE ( 'NONE', *, *, #12120, .F. ) ;
#16960 = AXIS2_PLACEMENT_3D ( 'NONE', #8012, #4228, #18200 ) ;
#16961 = ITEM_DEFINED_TRANSFORMATION ( 'NONE', 'NONE', #1431,  #18273 ) ;
#16962 = EDGE_LOOP ( 'NONE', ( #12069, #12903, #4015, #12689 ) ) ;
#16963 = CARTESIAN_POINT ( 'NONE',  ( -4.918774254215746211, 31.11359284679371484, -2.999999999999971578 ) ) ;
#16964 = CARTESIAN_POINT ( 'NONE',  ( 9.327259721468506015, -2.742977016014770175, 53.40697688051272962 ) ) ;
#16965 = CARTESIAN_POINT ( 'NONE',  ( -35.00000000000000000, 13.99999999999999822, 2.255140518769849223E-14 ) ) ;
#16966 = PLANE ( 'NONE',  #7601 ) ;
#16967 = LINE ( 'NONE', #20638, #690 ) ;
#16968 = ORIENTED_EDGE ( 'NONE', *, *, #21678, .F. ) ;
#16969 = DIRECTION ( 'NONE',  ( 0.000000000000000000, 0.000000000000000000, 1.000000000000000000 ) ) ;
#16970 = DIRECTION ( 'NONE',  ( -1.000000000000000000, -1.208970125616044077E-17, 0.000000000000000000 ) ) ;
#16971 = EDGE_LOOP ( 'NONE', ( #4594, #19392, #11798, #17015, #13953, #12460 ) ) ;
#16972 = CARTESIAN_POINT ( 'NONE',  ( -7.980461308159769729, 36.39375341857517299, 3.000000000000023537 ) ) ;
#16973 = CARTESIAN_POINT ( 'NONE',  ( 6.041077103370438905, -0.8288449397156273379, -52.13906252460637347 ) ) ;
#16974 = CARTESIAN_POINT ( 'NONE',  ( -34.99999999999999289, -5.000000000000000000, -5.000000000000030198 ) ) ;
#16975 = CIRCLE ( 'NONE', #18065, 2.000000000000002665 ) ;
#16976 = CARTESIAN_POINT ( 'NONE',  ( 6.631891271510764518, 39.71688159335408130, 53.15285333858339101 ) ) ;
#16977 = ORIENTED_EDGE ( 'NONE', *, *, #1714, .T. ) ;
#16978 = CARTESIAN_POINT ( 'NONE',  ( -90.00000000000000000, 40.00000000000000711, -9.108981535246192915E-16 ) ) ;
#16979 = EDGE_CURVE ( 'NONE', #6211, #14813, #7757, .T. ) ;
#16980 = ORIENTED_EDGE ( 'NONE', *, *, #19282, .T. ) ;
#16981 = FACE_OUTER_BOUND ( 'NONE', #17141, .T. ) ;
#16982 = ORIENTED_EDGE ( 'NONE', *, *, #3449, .T. ) ;
#16983 = CARTESIAN_POINT ( 'NONE',  ( 31.92986134326233838, -18.22261011550282817, 2.800654218530512551 ) ) ;
#16984 = AXIS2_PLACEMENT_3D ( 'NONE', #19012, #6628, #21998 ) ;
#16985 = DIRECTION ( 'NONE',  ( 6.505213034913038160E-19, 3.903127820947822896E-18, 1.000000000000000000 ) ) ;
#16986 = CARTESIAN_POINT ( 'NONE',  ( 3.330669073875469621E-13, -1.110223024625156540E-13, -2.999999999999971578 ) ) ;
#16987 = ADVANCED_FACE ( 'NONE', ( #12507 ), #1776, .F. ) ;
#16988 = CARTESIAN_POINT ( 'NONE',  ( 19.48215071167051704, 15.15508441932860606, -58.00945324419101468 ) ) ;
#16989 = ORIENTED_EDGE ( 'NONE', *, *, #15752, .T. ) ;
#16990 = ORIENTED_EDGE ( 'NONE', *, *, #9652, .T. ) ;
#16991 = VECTOR ( 'NONE', #3470, 1000.000000000000000 ) ;
#16992 = ORIENTED_EDGE ( 'NONE', *, *, #13764, .T. ) ;
#16993 = DIRECTION ( 'NONE',  ( 1.000000000000000000, 0.000000000000000000, 0.000000000000000000 ) ) ;
#16994 = VERTEX_POINT ( 'NONE', #3497 ) ;
#16995 = DIRECTION ( 'NONE',  ( 1.000000000000000000, 0.000000000000000000, 0.000000000000000000 ) ) ;
#16996 = CIRCLE ( 'NONE', #19571, 31.50000000000001421 ) ;
#16997 = CARTESIAN_POINT ( 'NONE',  ( 3.330669073875469621E-13, -1.110223024625156540E-13, -2.999999999999971578 ) ) ;
#16998 = EDGE_LOOP ( 'NONE', ( #717, #1671, #6647, #7494 ) ) ;
#16999 = DIRECTION ( 'NONE',  ( 0.000000000000000000, 0.000000000000000000, 1.000000000000000000 ) ) ;
#17000 = CARTESIAN_POINT ( 'NONE',  ( -7.480086125713259371, -0.2526605362823695633, -53.02285530597750807 ) ) ;
#17001 = ORIENTED_EDGE ( 'NONE', *, *, #16432, .T. ) ;
#17002 = CARTESIAN_POINT ( 'NONE',  ( -0.7921581640248792633, 13.00083933661134417, 6.999720221269573273 ) ) ;
#17003 = EDGE_CURVE ( 'NONE', #4421, #21115, #21161, .T. ) ;
#17004 = ORIENTED_EDGE ( 'NONE', *, *, #3060, .F. ) ;
#17005 = DIRECTION ( 'NONE',  ( 6.505213034913038160E-19, 3.903127820947822896E-18, 1.000000000000000000 ) ) ;
#17006 = CARTESIAN_POINT ( 'NONE',  ( 35.00000000000000000, -9.000000000000001776, -13.99999999999999645 ) ) ;
#17007 = CARTESIAN_POINT ( 'NONE',  ( -5.450915183833553575E-14, -3.671184582167058341, -46.55282949880530907 ) ) ;
#17008 = DIRECTION ( 'NONE',  ( 0.000000000000000000, 0.000000000000000000, -1.000000000000000000 ) ) ;
#17009 = VECTOR ( 'NONE', #16484, 1000.000000000000000 ) ;
#17010 = EDGE_CURVE ( 'NONE', #1089, #2580, #10914, .T. ) ;
#17011 = ADVANCED_FACE ( 'NONE', ( #21020 ), #17913, .T. ) ;
#17012 = CONICAL_SURFACE ( 'NONE', #6783, 49.99999999999998579, 0.7853981633974691512 ) ;
#17013 = CARTESIAN_POINT ( 'NONE',  ( -10.38220159744133042, 9.149172668433816824, 43.52345836121337896 ) ) ;
#17014 = VERTEX_POINT ( 'NONE', #19306 ) ;
#17015 = ORIENTED_EDGE ( 'NONE', *, *, #794, .T. ) ;
#17016 = EDGE_CURVE ( 'NONE', #1538, #14638, #2579, .T. ) ;
#17017 = ORIENTED_EDGE ( 'NONE', *, *, #3728, .T. ) ;
#17018 = AXIS2_PLACEMENT_3D ( 'NONE', #12906, #16586, #12571 ) ;
#17019 = ORIENTED_EDGE ( 'NONE', *, *, #12037, .F. ) ;
#17020 = CARTESIAN_POINT ( 'NONE',  ( -22.20813536596353188, 23.24072130216429599, 58.62062866457846866 ) ) ;
#17021 = DIRECTION ( 'NONE',  ( 1.000000000000000000, 1.208970125616053475E-17, 0.000000000000000000 ) ) ;
#17022 = VECTOR ( 'NONE', #10396, 1000.000000000000000 ) ;
#17023 = DIRECTION ( 'NONE',  ( 0.000000000000000000, 0.000000000000000000, -1.000000000000000000 ) ) ;
#17024 = CARTESIAN_POINT ( 'NONE',  ( -26.00000000000001421, 19.99999999999982947, -105.0010000000000048 ) ) ;
#17025 = AXIS2_PLACEMENT_3D ( 'NONE', #18412, #12901, #16701 ) ;
#17026 = DIRECTION ( 'NONE',  ( 0.000000000000000000, 0.000000000000000000, 1.000000000000000000 ) ) ;
#17027 = VERTEX_POINT ( 'NONE', #21465 ) ;
#17028 = CARTESIAN_POINT ( 'NONE',  ( -15.00000000000001421, 20.00000000000000355, 45.82575694955841072 ) ) ;
#17029 = DIRECTION ( 'NONE',  ( 0.000000000000000000, 0.000000000000000000, -1.000000000000000000 ) ) ;
#17030 = CARTESIAN_POINT ( 'NONE',  ( 47.83731665821556334, 7.000000000000000000, -38.93845529828706020 ) ) ;
#17031 = CARTESIAN_POINT ( 'NONE',  ( 11.15511648636531739, 39.11609166919075165, -55.07420106209022492 ) ) ;
#17032 = ORIENTED_EDGE ( 'NONE', *, *, #11411, .T. ) ;
#17033 = LINE ( 'NONE', #18659, #17935 ) ;
#17034 = AXIS2_PLACEMENT_3D ( 'NONE', #6424, #4824, #10070 ) ;
#17035 = AXIS2_PLACEMENT_3D ( 'NONE', #14372, #11056, #9228 ) ;
#17036 = ORIENTED_EDGE ( 'NONE', *, *, #13913, .F. ) ;
#17037 = CARTESIAN_POINT ( 'NONE',  ( 2.220446049250313081E-13, 2.775557561562891351E-14, -2.800654218530485018 ) ) ;
#17038 = DIRECTION ( 'NONE',  ( 0.000000000000000000, 0.000000000000000000, -1.000000000000000000 ) ) ;
#17039 = FACE_OUTER_BOUND ( 'NONE', #13292, .T. ) ;
#17040 = VECTOR ( 'NONE', #12142, 1000.000000000000000 ) ;
#17041 = EDGE_CURVE ( 'NONE', #2693, #5200, #4983, .T. ) ;
#17042 = VERTEX_POINT ( 'NONE', #4285 ) ;
#17043 = B_SPLINE_CURVE_WITH_KNOTS ( 'NONE', 3,
 ( #4286, #13411, #18477, #5992, #14688, #16644, #11257, #834, #22036, #6226, #949, #9436, #7714, #18255, #13185, #2566, #20434, #11490, #4625, #9547 ),
 .UNSPECIFIED., .F., .F.,
 ( 4, 2, 2, 2, 2, 2, 2, 2, 2, 4 ),
 ( 0.02328883130680912614, 0.02567687977621935236, 0.02687090401092445680, 0.02806492824562956817, 0.03284102518444999980, 0.03522907365386021561, 0.03761712212327043836, 0.03881114635797554280, 0.04000517059268065417, 0.04239321906209086999 ),
 .UNSPECIFIED. ) ;
#17044 = AXIS2_PLACEMENT_3D ( 'NONE', #12009, #6622, #9940 ) ;
#17045 = EDGE_CURVE ( 'NONE', #9285, #10824, #9670, .T. ) ;
#17046 = VERTEX_POINT ( 'NONE', #12743 ) ;
#17047 = CARTESIAN_POINT ( 'NONE',  ( 0.05615509895247599442, -4.650464140362338128, 45.38761122811000348 ) ) ;
#17048 = EDGE_CURVE ( 'NONE', #7486, #1875, #16320, .T. ) ;
#17049 = DIRECTION ( 'NONE',  ( -0.000000000000000000, -1.000000000000000000, -0.000000000000000000 ) ) ;
#17050 = AXIS2_PLACEMENT_3D ( 'NONE', #2885, #20744, #15107 ) ;
#17051 = CIRCLE ( 'NONE', #6830, 2.500000000000002220 ) ;
#17052 = AXIS2_PLACEMENT_3D ( 'NONE', #5511, #8733, #3586 ) ;
#17053 = ORIENTED_EDGE ( 'NONE', *, *, #22158, .T. ) ;
#17054 = CARTESIAN_POINT ( 'NONE',  ( 13.25963002225072884, 12.97669314386523176, 45.02656532858659943 ) ) ;
#17055 = CARTESIAN_POINT ( 'NONE',  ( -4.076028284552909220, 34.44346285612737546, -39.58813741008486886 ) ) ;
#17056 = CARTESIAN_POINT ( 'NONE',  ( 35.00000000000000000, 2.142135623730931471, -49.99999999999999289 ) ) ;
#17057 = CARTESIAN_POINT ( 'NONE',  ( -18.82278182890058460, 26.77493817624126038, -60.32982055024027801 ) ) ;
#17058 = CARTESIAN_POINT ( 'NONE',  ( -4.198142121831033968, 39.89210073658759370, 51.71386687473788868 ) ) ;
#17059 = AXIS2_PLACEMENT_3D ( 'NONE', #17949, #14033, #10496 ) ;
#17060 = ORIENTED_EDGE ( 'NONE', *, *, #6366, .F. ) ;
#17061 = CARTESIAN_POINT ( 'NONE',  ( 11.84374239103369497, 29.21200678190359667, 44.31542800769556578 ) ) ;
#17062 = DIRECTION ( 'NONE',  ( 1.296372316667914327E-16, 1.000000000000000000, -0.000000000000000000 ) ) ;
#17063 = CARTESIAN_POINT ( 'NONE',  ( 11.00126833636921830, 3.276569432483688704, -57.62199738645433200 ) ) ;
#17064 = CARTESIAN_POINT ( 'NONE',  ( 3.877306978638209416E-14, 1.500000000000004885, -12.00000000000000355 ) ) ;
#17065 = VERTEX_POINT ( 'NONE', #16642 ) ;
#17066 = CARTESIAN_POINT ( 'NONE',  ( 5.249999999999981348, 40.00000000000000000, 41.42387596543812123 ) ) ;
#17067 = CARTESIAN_POINT ( 'NONE',  ( -5.074925817841608122, 32.10132595304110481, 3.000000000000016431 ) ) ;
#17068 = CARTESIAN_POINT ( 'NONE',  ( 24.43568323314253021, -26.65040777864172838, 2.932460736555815739 ) ) ;
#17069 = CARTESIAN_POINT ( 'NONE',  ( 27.56232195404068008, -21.41958700883258970, 2.999999999999995559 ) ) ;
#17070 = VECTOR ( 'NONE', #14876, 1000.000000000000000 ) ;
#17071 = ORIENTED_EDGE ( 'NONE', *, *, #2211, .T. ) ;
#17072 = ORIENTED_EDGE ( 'NONE', *, *, #11553, .T. ) ;
#17073 = ORIENTED_EDGE ( 'NONE', *, *, #21981, .T. ) ;
#17074 = DIRECTION ( 'NONE',  ( 0.000000000000000000, 0.000000000000000000, 1.000000000000000000 ) ) ;
#17075 = CARTESIAN_POINT ( 'NONE',  ( 34.99999999999999289, -5.000000000000000000, -57.49999999999705835 ) ) ;
#17076 = LINE ( 'NONE', #5286, #6270 ) ;
#17077 = CARTESIAN_POINT ( 'NONE',  ( 16.07406985629799578, 8.092854060485286993, 59.53272467997607720 ) ) ;
#17078 = DIRECTION ( 'NONE',  ( -6.505213034913038160E-19, -3.903127820947822896E-18, -1.000000000000000000 ) ) ;
#17079 = CIRCLE ( 'NONE', #5029, 3.999999999999998224 ) ;
#17080 = ORIENTED_EDGE ( 'NONE', *, *, #3080, .F. ) ;
#17081 = DIRECTION ( 'NONE',  ( 1.000000000000000000, 0.000000000000000000, 0.000000000000000000 ) ) ;
#17082 = DIRECTION ( 'NONE',  ( 6.505213034913038160E-19, 3.903127820947822896E-18, 1.000000000000000000 ) ) ;
#17083 = ORIENTED_EDGE ( 'NONE', *, *, #21587, .F. ) ;
#17084 = DIRECTION ( 'NONE',  ( -1.000000000000000000, 1.264902534566421922E-16, 0.000000000000000000 ) ) ;
#17085 = AXIS2_PLACEMENT_3D ( 'NONE', #21074, #20858, #12354 ) ;
#17086 = EDGE_CURVE ( 'NONE', #10900, #18746, #1070, .T. ) ;
#17087 = CARTESIAN_POINT ( 'NONE',  ( 7.577104390338814888, -0.4826542685309015424, -53.01683071947938686 ) ) ;
#17088 = DIRECTION ( 'NONE',  ( 6.505213034913038160E-19, 3.903127820947822896E-18, 1.000000000000000000 ) ) ;
#17089 = CARTESIAN_POINT ( 'NONE',  ( 4.196817044553720066, 39.89217751381926291, 51.71303682859505102 ) ) ;
#17090 = ORIENTED_EDGE ( 'NONE', *, *, #17996, .F. ) ;
#17091 = CARTESIAN_POINT ( 'NONE',  ( 13.08927703801863807, 27.36553638769442998, -44.94509734929665967 ) ) ;
#17092 = ORIENTED_EDGE ( 'NONE', *, *, #5691, .T. ) ;
#17093 = DIRECTION ( 'NONE',  ( -0.000000000000000000, -0.000000000000000000, -1.000000000000000000 ) ) ;
#17094 = CARTESIAN_POINT ( 'NONE',  ( -22.42598460344824218, 19.26775710289567201, 58.66769746720327561 ) ) ;
#17095 = VERTEX_POINT ( 'NONE', #4167 ) ;
#17096 = CARTESIAN_POINT ( 'NONE',  ( 5.833333333333329485, 40.00000000000000000, -40.61164310337066041 ) ) ;
#17097 = ADVANCED_FACE ( 'NONE', ( #2565 ), #14796, .F. ) ;
#17098 = DIRECTION ( 'NONE',  ( 1.209647751973867239E-17, 1.000000000000000000, -3.903127820947822896E-18 ) ) ;
#17099 = CARTESIAN_POINT ( 'NONE',  ( 24.73600648735124707, -27.19760187735892387, -2.800654218530457484 ) ) ;
#17100 = VECTOR ( 'NONE', #9877, 1000.000000000000000 ) ;
#17101 = CARTESIAN_POINT ( 'NONE',  ( 20.32373648405300770, 10.46972314276608884, -58.17772014969877148 ) ) ;
#17102 = CONICAL_SURFACE ( 'NONE', #9452, 20.00000000000002132, 0.7853981633974543852 ) ;
#17103 = ORIENTED_EDGE ( 'NONE', *, *, #8149, .F. ) ;
#17104 = ORIENTED_EDGE ( 'NONE', *, *, #15162, .T. ) ;
#17105 = ORIENTED_EDGE ( 'NONE', *, *, #5361, .T. ) ;
#17106 = EDGE_LOOP ( 'NONE', ( #6711, #21268, #1265, #9563 ) ) ;
#17107 = CARTESIAN_POINT ( 'NONE',  ( -34.99999999999999289, 5.000000000000000000, -3.012171160963566127E-14 ) ) ;
#17108 = DIRECTION ( 'NONE',  ( 0.000000000000000000, 0.000000000000000000, -1.000000000000000000 ) ) ;
#17109 = DIRECTION ( 'NONE',  ( 1.000000000000000000, 0.000000000000000000, 0.000000000000000000 ) ) ;
#17110 = AXIS2_PLACEMENT_3D ( 'NONE', #4835, #11807, #9762 ) ;
#17111 = ORIENTED_EDGE ( 'NONE', *, *, #9752, .F. ) ;
#17112 = DIRECTION ( 'NONE',  ( 0.9659258262890679791, -0.2588190451025219052, 0.000000000000000000 ) ) ;
#17113 = CARTESIAN_POINT ( 'NONE',  ( 2.999999999999998668, 15.99999999999999645, 6.485281374238567764 ) ) ;
#17114 = ORIENTED_EDGE ( 'NONE', *, *, #1151, .T. ) ;
#17115 = ADVANCED_FACE ( 'NONE', ( #16416 ), #7597, .F. ) ;
#17116 = ORIENTED_EDGE ( 'NONE', *, *, #2880, .T. ) ;
#17117 = DIRECTION ( 'NONE',  ( -1.000000000000000000, 1.084202172485504681E-16, 0.000000000000000000 ) ) ;
#17118 = CIRCLE ( 'NONE', #13085, 2.500000000000008882 ) ;
#17119 = CARTESIAN_POINT ( 'NONE',  ( 42.50000000000000711, -12.00000000000000000, 54.00000000000000711 ) ) ;
#17120 = DIRECTION ( 'NONE',  ( 0.000000000000000000, 1.000000000000000000, 0.000000000000000000 ) ) ;
#17121 = CIRCLE ( 'NONE', #21155, 2.499999999999998668 ) ;
#17122 = CARTESIAN_POINT ( 'NONE',  ( 24.79619811426220366, -21.00948735876903584, -6.999999999999950262 ) ) ;
#17123 = DIRECTION ( 'NONE',  ( -6.505213034913038160E-19, -3.903127820947822896E-18, -1.000000000000000000 ) ) ;
#17124 = CARTESIAN_POINT ( 'NONE',  ( 7.505578006075174891, 1.461761173328240071, -55.63523492904086254 ) ) ;
#17125 = CIRCLE ( 'NONE', #7983, 2.099999999999997868 ) ;
#17126 = VERTEX_POINT ( 'NONE', #6223 ) ;
#17127 = CIRCLE ( 'NONE', #1409, 49.99999999999998579 ) ;
#17128 = CIRCLE ( 'NONE', #11659, 4.025000000000000355 ) ;
#17129 = EDGE_LOOP ( 'NONE', ( #19645, #4186, #2059, #3235, #18733, #505 ) ) ;
#17130 = ADVANCED_FACE ( 'NONE', ( #5884 ), #11141, .T. ) ;
#17131 = EDGE_LOOP ( 'NONE', ( #19933, #4255, #10024 ) ) ;
#17132 = CIRCLE ( 'NONE', #20077, 0.9999999999999956701 ) ;
#17133 = VERTEX_POINT ( 'NONE', #21694 ) ;
#17134 = CARTESIAN_POINT ( 'NONE',  ( -31.41239365194190114, 2.347663744114103501, -7.000000000000006217 ) ) ;
#17135 = DIRECTION ( 'NONE',  ( 6.505213034913038160E-19, 3.903127820947822896E-18, 1.000000000000000000 ) ) ;
#17136 = CARTESIAN_POINT ( 'NONE',  ( 2.232799048558932853, 39.96997190553584289, -50.39091384480168756 ) ) ;
#17137 = CARTESIAN_POINT ( 'NONE',  ( -17.38288706075493906, 10.07729229769342538, -59.93358289200955369 ) ) ;
#17138 = DIRECTION ( 'NONE',  ( 6.505213034913038160E-19, 3.903127820947822896E-18, 1.000000000000000000 ) ) ;
#17139 = EDGE_CURVE ( 'NONE', #7962, #17550, #9375, .T. ) ;
#17140 = EDGE_CURVE ( 'NONE', #16507, #5122, #16681, .T. ) ;
#17141 = EDGE_LOOP ( 'NONE', ( #17111, #9155, #1427, #6933 ) ) ;
#17142 = DIRECTION ( 'NONE',  ( 0.1421319796954317316, 0.000000000000000000, 0.9898477157360405787 ) ) ;
#17143 = CARTESIAN_POINT ( 'NONE',  ( -8.743619476591407036, 40.00000000000000000, -53.24632774931270518 ) ) ;
#17144 = CIRCLE ( 'NONE', #316, 4.000000000000145661 ) ;
#17145 = PLANE ( 'NONE',  #4704 ) ;
#17146 = DIRECTION ( 'NONE',  ( -1.000000000000000000, 0.000000000000000000, -0.000000000000000000 ) ) ;
#17147 = ORIENTED_EDGE ( 'NONE', *, *, #903, .F. ) ;
#17148 = EDGE_CURVE ( 'NONE', #20269, #10746, #3884, .T. ) ;
#17149 = LINE ( 'NONE', #1463, #13879 ) ;
#17150 =( GEOMETRIC_REPRESENTATION_CONTEXT ( 3 ) GLOBAL_UNCERTAINTY_ASSIGNED_CONTEXT ( ( #16772 ) ) GLOBAL_UNIT_ASSIGNED_CONTEXT ( ( #7360, #14326, #5755 ) ) REPRESENTATION_CONTEXT ( 'NONE', 'WORKASPACE' ) );
#17151 = ORIENTED_EDGE ( 'NONE', *, *, #13922, .T. ) ;
#17152 = DIRECTION ( 'NONE',  ( -6.505213034913038160E-19, -3.903127820947822896E-18, -1.000000000000000000 ) ) ;
#17153 = CYLINDRICAL_SURFACE ( 'NONE', #6031, 36.76383501243555685 ) ;
#17154 = DIRECTION ( 'NONE',  ( 1.000000000000000000, 0.000000000000000000, 0.000000000000000000 ) ) ;
#17155 = ADVANCED_FACE ( 'NONE', ( #3012 ), #20644, .T. ) ;
#17156 = ORIENTED_EDGE ( 'NONE', *, *, #16598, .F. ) ;
#17157 = EDGE_CURVE ( 'NONE', #18373, #8686, #17309, .T. ) ;
#17158 = AXIS2_PLACEMENT_3D ( 'NONE', #4431, #17008, #4660 ) ;
#17159 = AXIS2_PLACEMENT_3D ( 'NONE', #11025, #5763, #14682 ) ;
#17160 = ORIENTED_EDGE ( 'NONE', *, *, #18855, .T. ) ;
#17161 = FACE_OUTER_BOUND ( 'NONE', #16013, .T. ) ;
#17162 = DIRECTION ( 'NONE',  ( 6.505213034913038160E-19, 3.903127820947822896E-18, 1.000000000000000000 ) ) ;
#17163 = EDGE_CURVE ( 'NONE', #8686, #13563, #12300, .T. ) ;
#17164 = ORIENTED_EDGE ( 'NONE', *, *, #13581, .T. ) ;
#17165 = CARTESIAN_POINT ( 'NONE',  ( 8.199064559763613147, 7.360541284256825634, 42.22991907770642683 ) ) ;
#17166 = CARTESIAN_POINT ( 'NONE',  ( -3.601266574137734100, 34.57013445913566585, -39.39030536259064519 ) ) ;
#17167 = CARTESIAN_POINT ( 'NONE',  ( -13.00000000000000178, 20.00000000000000000, -11.32475165290611407 ) ) ;
#17168 = CARTESIAN_POINT ( 'NONE',  ( -21.72501817863217966, 25.59362490671916746, -58.51313831023544765 ) ) ;
#17169 = EDGE_CURVE ( 'NONE', #4759, #21174, #369, .T. ) ;
#17170 = DIRECTION ( 'NONE',  ( 1.000000000000000000, 0.000000000000000000, 0.000000000000000000 ) ) ;
#17171 = CARTESIAN_POINT ( 'NONE',  ( -13.10473755708775201, 38.28578281281269113, 55.88243319223045091 ) ) ;
#17172 = VECTOR ( 'NONE', #5329, 1000.000000000000000 ) ;
#17173 = VERTEX_POINT ( 'NONE', #4952 ) ;
#17174 = CARTESIAN_POINT ( 'NONE',  ( 14.92530643917652711, 21.54450079162174703, 45.79309713780077118 ) ) ;
#17175 = CARTESIAN_POINT ( 'NONE',  ( -1.387778780781445518E-14, 20.00000000000000355, 105.0000000000000142 ) ) ;
#17176 = EDGE_CURVE ( 'NONE', #12190, #21043, #969, .T. ) ;
#17177 = CARTESIAN_POINT ( 'NONE',  ( 6.000000000000000888, 0.000000000000000000, 6.000000000000000000 ) ) ;
#17178 = CYLINDRICAL_SURFACE ( 'NONE', #7804, 2.500000000000002220 ) ;
#17179 = VERTEX_POINT ( 'NONE', #15018 ) ;
#17180 = EDGE_CURVE ( 'NONE', #10912, #16627, #6089, .T. ) ;
#17181 = ADVANCED_FACE ( 'NONE', ( #1282, #12053 ), #20317, .F. ) ;
#17182 = DIRECTION ( 'NONE',  ( 6.505213034913038160E-19, 3.903127820947822896E-18, 1.000000000000000000 ) ) ;
#17183 = DIRECTION ( 'NONE',  ( -6.505213034913038160E-19, -3.903127820947822896E-18, -1.000000000000000000 ) ) ;
#17184 = B_SPLINE_CURVE_WITH_KNOTS ( 'NONE', 3,
 ( #19274, #13964, #1512, #12157 ),
 .UNSPECIFIED., .F., .F.,
 ( 4, 4 ),
 ( 0.001875451646903196793, 0.003761979286331223853 ),
 .UNSPECIFIED. ) ;
#17185 = VERTEX_POINT ( 'NONE', #11931 ) ;
#17186 = CIRCLE ( 'NONE', #12785, 16.49999999999998579 ) ;
#17187 = APPLICATION_PROTOCOL_DEFINITION ( 'draft international standard', 'automotive_design', 1998, #6086 ) ;
#17188 = ORIENTED_EDGE ( 'NONE', *, *, #5747, .F. ) ;
#17189 = DIRECTION ( 'NONE',  ( 0.000000000000000000, -1.000000000000000000, 0.000000000000000000 ) ) ;
#17190 = CARTESIAN_POINT ( 'NONE',  ( -0.6864184775319864817, -1.216838870810144080, 47.75834167804403307 ) ) ;
#17191 = CARTESIAN_POINT ( 'NONE',  ( 0.000000000000000000, 30.00000000000000000, 0.000000000000000000 ) ) ;
#17192 = CARTESIAN_POINT ( 'NONE',  ( 15.62726112422616076, 28.45046755804878202, 2.999999999999995559 ) ) ;
#17193 = DIRECTION ( 'NONE',  ( -0.000000000000000000, 1.000000000000000000, -0.000000000000000000 ) ) ;
#17194 = ORIENTED_EDGE ( 'NONE', *, *, #15397, .T. ) ;
#17195 = CARTESIAN_POINT ( 'NONE',  ( -35.00000000000000000, -9.000000000000001776, 1.387778780781445676E-14 ) ) ;
#17196 = DIRECTION ( 'NONE',  ( 0.000000000000000000, 0.000000000000000000, 1.000000000000000000 ) ) ;
#17197 = ORIENTED_EDGE ( 'NONE', *, *, #10353, .T. ) ;
#17198 = CARTESIAN_POINT ( 'NONE',  ( -36.06598984771573413, 7.000000000000000000, 48.42385786802029912 ) ) ;
#17199 = ADVANCED_FACE ( 'NONE', ( #18932 ), #6445, .T. ) ;
#17200 = CARTESIAN_POINT ( 'NONE',  ( -18.65063509461084479, 12.49999999999990052, 3.000000000000023537 ) ) ;
#17201 = CARTESIAN_POINT ( 'NONE',  ( 35.79662727779919607, -4.171001175319821286, -2.999999999999971578 ) ) ;
#17202 = CARTESIAN_POINT ( 'NONE',  ( 9.506747383188477230, 40.00000000000000711, 53.50938557514125193 ) ) ;
#17203 = ORIENTED_EDGE ( 'NONE', *, *, #17041, .T. ) ;
#17204 = CARTESIAN_POINT ( 'NONE',  ( 12.06668108811418705, 28.91809087000033784, -44.43106897542662637 ) ) ;
#17205 = VERTEX_POINT ( 'NONE', #22034 ) ;
#17206 = CARTESIAN_POINT ( 'NONE',  ( 1.243967489023766193, -3.588031564569214659E-15, -51.43875557960451061 ) ) ;
#17207 = CARTESIAN_POINT ( 'NONE',  ( -20.36304159388344104, -24.03323817228492132, -6.999999999999950262 ) ) ;
#17208 = EDGE_LOOP ( 'NONE', ( #12649, #11412, #17539, #3889, #10111, #8852, #6580, #18747, #6663, #5787, #1658, #229, #3362, #22512, #19939, #11676 ) ) ;
#17209 = DIRECTION ( 'NONE',  ( 0.000000000000000000, 0.000000000000000000, -1.000000000000000000 ) ) ;
#17210 = EDGE_CURVE ( 'NONE', #6573, #17126, #21835, .T. ) ;
#17211 = DIRECTION ( 'NONE',  ( 1.296372316667914327E-16, 1.000000000000000000, -0.000000000000000000 ) ) ;
#17212 = CARTESIAN_POINT ( 'NONE',  ( 32.20238537491837150, 4.080045426412631571, -2.999999999999975131 ) ) ;
#17213 = CARTESIAN_POINT ( 'NONE',  ( 5.999999999999999112, 0.000000000000000000, -6.000000000000000000 ) ) ;
#17215 = VERTEX_POINT ( 'NONE', #17200 ) ;
#17214 = EDGE_CURVE ( 'NONE', #13845, #2563, #4997, .T. ) ;
#17216 = VECTOR ( 'NONE', #18347, 1000.000000000000000 ) ;
#17217 = VERTEX_POINT ( 'NONE', #8164 ) ;
#17218 = ORIENTED_EDGE ( 'NONE', *, *, #22366, .T. ) ;
#17219 = CARTESIAN_POINT ( 'NONE',  ( 3.849727973822421485E-15, 1.499999999999997780, 0.000000000000000000 ) ) ;
#17220 = EDGE_LOOP ( 'NONE', ( #14722, #8482, #140, #558 ) ) ;
#17221 = CARTESIAN_POINT ( 'NONE',  ( -4.170748987303213084, 34.65667543218822999, 3.000000000000002665 ) ) ;
#17222 = CARTESIAN_POINT ( 'NONE',  ( 14.71244060472245252, 36.96434927850640406, 56.47085971327723541 ) ) ;
#17223 = EDGE_CURVE ( 'NONE', #10226, #7247, #22149, .T. ) ;
#17224 = FACE_BOUND ( 'NONE', #1556, .T. ) ;
#17225 = ORIENTED_EDGE ( 'NONE', *, *, #3623, .F. ) ;
#17226 = DIRECTION ( 'NONE',  ( 0.000000000000000000, -1.000000000000000000, 0.000000000000000000 ) ) ;
#17227 = CARTESIAN_POINT ( 'NONE',  ( 1.564319729173993423, -1.162775034690379128, -47.08282483555583298 ) ) ;
#17228 = EDGE_LOOP ( 'NONE', ( #5235, #19522, #8955, #9281 ) ) ;
#17229 = CARTESIAN_POINT ( 'NONE',  ( -6.093892532912075666, 0.8902119804445677298, 54.73806350723837966 ) ) ;
#17230 = CARTESIAN_POINT ( 'NONE',  ( 6.000000000000000888, -40.00000000000000000, 6.000000000000000000 ) ) ;
#17231 = ORIENTED_EDGE ( 'NONE', *, *, #9302, .T. ) ;
#17232 = CARTESIAN_POINT ( 'NONE',  ( -13.00000000000000000, -20.00000000000000000, -11.32475165290611230 ) ) ;
#17233 = DIRECTION ( 'NONE',  ( 0.000000000000000000, 0.000000000000000000, -1.000000000000000000 ) ) ;
#17234 = CARTESIAN_POINT ( 'NONE',  ( -0.5261157918504695274, 39.99836265446453609, 49.13909455355741329 ) ) ;
#17235 = AXIS2_PLACEMENT_3D ( 'NONE', #11593, #22026, #13279 ) ;
#17236 = CARTESIAN_POINT ( 'NONE',  ( 9.708269511265410046, -33.52953626616050542, -2.999999999999971578 ) ) ;
#17238 = ORIENTED_EDGE ( 'NONE', *, *, #1765, .T. ) ;
#17237 = ADVANCED_FACE ( 'NONE', ( #20432 ), #18708, .F. ) ;
#17239 = CIRCLE ( 'NONE', #20924, 18.00000000000000355 ) ;
#17240 = AXIS2_PLACEMENT_3D ( 'NONE', #9872, #2666, #6214 ) ;
#17241 = PRODUCT_DEFINITION ( 'UNKNOWN', '', #21568, #409 ) ;
#17242 = ORIENTED_EDGE ( 'NONE', *, *, #20748, .T. ) ;
#17243 = ORIENTED_EDGE ( 'NONE', *, *, #1708, .T. ) ;
#17244 = B_SPLINE_CURVE_WITH_KNOTS ( 'NONE', 3,
 ( #11176, #14378, #4204, #7745 ),
 .UNSPECIFIED., .F., .F.,
 ( 4, 4 ),
 ( 0.001893031756885613093, 0.003808480026563617130 ),
 .UNSPECIFIED. ) ;
#17245 = VERTEX_POINT ( 'NONE', #22380 ) ;
#17246 = DIRECTION ( 'NONE',  ( 0.000000000000000000, 0.000000000000000000, 1.000000000000000000 ) ) ;
#17247 = EDGE_CURVE ( 'NONE', #2560, #19747, #12660, .T. ) ;
#17248 = CARTESIAN_POINT ( 'NONE',  ( -11.86180952234344588, 38.99999999999292299, 55.35904751185378103 ) ) ;
#17249 = DIRECTION ( 'NONE',  ( 0.000000000000000000, 0.000000000000000000, 1.000000000000000000 ) ) ;
#17250 = CARTESIAN_POINT ( 'NONE',  ( -12.92329681834244681, 4.659497110088497429, -58.43073491095716321 ) ) ;
#17251 = CARTESIAN_POINT ( 'NONE',  ( 0.2640866558584379353, 39.99958921855358795, 48.93844575723053936 ) ) ;
#17252 = EDGE_LOOP ( 'NONE', ( #4079, #3053, #12398, #19917 ) ) ;
#17253 = FACE_OUTER_BOUND ( 'NONE', #20361, .T. ) ;
#17254 = CARTESIAN_POINT ( 'NONE',  ( -9.100109617798446848, 40.00000000000000000, -53.37249913072469099 ) ) ;
#17255 = DIRECTION ( 'NONE',  ( -6.505213034913038160E-19, -3.903127820947822896E-18, -1.000000000000000000 ) ) ;
#17256 = CARTESIAN_POINT ( 'NONE',  ( -17.99805307122272069, -21.44924440733175786, -2.999999999999971578 ) ) ;
#17257 =( LENGTH_UNIT ( ) NAMED_UNIT ( * ) SI_UNIT ( .MILLI., .METRE. ) );
#17258 = VECTOR ( 'NONE', #18332, 1000.000000000000000 ) ;
#17259 = ADVANCED_FACE ( 'NONE', ( #22491 ), #2054, .T. ) ;
#17260 = VERTEX_POINT ( 'NONE', #3355 ) ;
#17261 = CARTESIAN_POINT ( 'NONE',  ( 35.00000000000000000, 22.00000000000000355, 2.365113165210053967E-14 ) ) ;
#17262 = ORIENTED_EDGE ( 'NONE', *, *, #2852, .F. ) ;
#17263 = DIRECTION ( 'NONE',  ( -1.000000000000000000, -1.208970125616046080E-17, 6.505213034913038160E-19 ) ) ;
#17264 = CARTESIAN_POINT ( 'NONE',  ( 34.99999999999980815, 40.00000000000000711, 54.99999999999922551 ) ) ;
#17265 = DIRECTION ( 'NONE',  ( -1.296372316667914327E-16, -1.000000000000000000, 0.000000000000000000 ) ) ;
#17266 = EDGE_CURVE ( 'NONE', #9068, #105, #9009, .T. ) ;
#17267 = ORIENTED_EDGE ( 'NONE', *, *, #356, .F. ) ;
#17268 = ORIENTED_EDGE ( 'NONE', *, *, #15483, .T. ) ;
#17269 = CARTESIAN_POINT ( 'NONE',  ( 9.079900084793775861, 0.2952492082908232396, -53.92155889450892658 ) ) ;
#17270 = CIRCLE ( 'NONE', #1923, 36.76383501243555685 ) ;
#17271 = DIRECTION ( 'NONE',  ( 1.000000000000000000, 0.000000000000000000, -1.224646799147353207E-16 ) ) ;
#17272 = EDGE_LOOP ( 'NONE', ( #6672, #13882, #12444, #14063 ) ) ;
#17273 = CARTESIAN_POINT ( 'NONE',  ( 10.38193264731104115, 9.167449762519604306, 43.52061562521062399 ) ) ;
#17274 = CARTESIAN_POINT ( 'NONE',  ( -5.999999999999999112, -40.00000000000000000, 6.000000000000001776 ) ) ;
#17275 = DIRECTION ( 'NONE',  ( 0.000000000000000000, -0.7071067811865500152, -0.7071067811865451302 ) ) ;
#17276 = CARTESIAN_POINT ( 'NONE',  ( -21.77460018174987155, 14.53841458819381316, -58.52494103856261631 ) ) ;
#17277 = DIRECTION ( 'NONE',  ( 0.000000000000000000, 0.000000000000000000, 1.000000000000000000 ) ) ;
#17278 = ADVANCED_FACE ( 'NONE', ( #8941 ), #19160, .T. ) ;
#17279 = VERTEX_POINT ( 'NONE', #21101 ) ;
#17280 = FACE_OUTER_BOUND ( 'NONE', #15112, .T. ) ;
#17281 = DIRECTION ( 'NONE',  ( 0.000000000000000000, 0.000000000000000000, 1.000000000000000000 ) ) ;
#17282 = CARTESIAN_POINT ( 'NONE',  ( -42.50000000000000711, -12.00000000000012434, 44.97499999999989484 ) ) ;
#17283 = CARTESIAN_POINT ( 'NONE',  ( 2.220446049250313081E-13, -8.326672684688674053E-14, 2.800654218530498785 ) ) ;
#17284 = AXIS2_PLACEMENT_3D ( 'NONE', #14984, #13037, #4586 ) ;
#17285 = ORIENTED_EDGE ( 'NONE', *, *, #9735, .F. ) ;
#17286 = CIRCLE ( 'NONE', #16564, 19.99999999999999289 ) ;
#17287 = CARTESIAN_POINT ( 'NONE',  ( -7.463862311151175710, -35.99819890246952525, -2.800654218530457484 ) ) ;
#17288 = DIRECTION ( 'NONE',  ( 0.000000000000000000, -1.000000000000000000, 0.000000000000000000 ) ) ;
#17289 = LINE ( 'NONE', #22472, #16408 ) ;
#17290 = EDGE_CURVE ( 'NONE', #10462, #17245, #20727, .T. ) ;
#17291 = EDGE_CURVE ( 'NONE', #17046, #5486, #3855, .T. ) ;
#17292 = AXIS2_PLACEMENT_3D ( 'NONE', #5331, #21141, #17689 ) ;
#17293 = EDGE_CURVE ( 'NONE', #16794, #2875, #5400, .T. ) ;
#17294 = ORIENTED_EDGE ( 'NONE', *, *, #19808, .T. ) ;
#17295 = ADVANCED_FACE ( 'NONE', ( #19389 ), #7111, .T. ) ;
#17296 = APPLICATION_PROTOCOL_DEFINITION ( 'draft international standard', 'automotive_design', 1998, #16165 ) ;
#17297 = ORIENTED_EDGE ( 'NONE', *, *, #18071, .T. ) ;
#17298 = CYLINDRICAL_SURFACE ( 'NONE', #21277, 6.499999999999999112 ) ;
#17299 = DIRECTION ( 'NONE',  ( 0.000000000000000000, 0.000000000000000000, -1.000000000000000000 ) ) ;
#17300 = CIRCLE ( 'NONE', #109, 34.90673715956759082 ) ;
#17301 = DIRECTION ( 'NONE',  ( 1.000000000000000000, 0.000000000000000000, 0.000000000000000000 ) ) ;
#17302 = VERTEX_POINT ( 'NONE', #3693 ) ;
#17303 = DIRECTION ( 'NONE',  ( -0.000000000000000000, -1.000000000000000000, -0.000000000000000000 ) ) ;
#17304 = MECHANICAL_DESIGN_GEOMETRIC_PRESENTATION_REPRESENTATION (  '', ( #7851 ), #13264 ) ;
#17305 = CARTESIAN_POINT ( 'NONE',  ( -11.86180952234070674, 38.99999999999457145, 55.35904751185264416 ) ) ;
#17306 = EDGE_LOOP ( 'NONE', ( #3475, #10052, #17557, #8558 ) ) ;
#17307 = DIRECTION ( 'NONE',  ( -0.000000000000000000, -0.000000000000000000, -1.000000000000000000 ) ) ;
#17308 = AXIS2_PLACEMENT_3D ( 'NONE', #15374, #10437, #6681 ) ;
#17309 = LINE ( 'NONE', #13524, #22558 ) ;
#17310 = CARTESIAN_POINT ( 'NONE',  ( -9.165151389911724067, 39.99999999999999289, -56.36098470834080132 ) ) ;
#17311 = CARTESIAN_POINT ( 'NONE',  ( 3.019668934335359545, 39.94555832490831193, 50.93804378708211544 ) ) ;
#17312 = CARTESIAN_POINT ( 'NONE',  ( 8.188149873056865147, 32.58630821608367256, -42.20917188641860207 ) ) ;
#17313 = ORIENTED_EDGE ( 'NONE', *, *, #17534, .F. ) ;
#17314 = CARTESIAN_POINT ( 'NONE',  ( 6.696867368503558448E-15, 40.00000000000000000, 48.73397172404481381 ) ) ;
#17315 = CARTESIAN_POINT ( 'NONE',  ( 35.00000000000001421, 14.00000000000000000, 39.00000000000002132 ) ) ;
#17316 = ORIENTED_EDGE ( 'NONE', *, *, #3376, .F. ) ;
#17317 = FACE_OUTER_BOUND ( 'NONE', #16762, .T. ) ;
#17318 = CIRCLE ( 'NONE', #9273, 36.76383501243555685 ) ;
#17319 = LINE ( 'NONE', #8617, #21056 ) ;
#17320 = CARTESIAN_POINT ( 'NONE',  ( 32.40961249803578426, -2.422192751864227223, -2.999999999999981792 ) ) ;
#17321 = AXIS2_PLACEMENT_3D ( 'NONE', #3971, #5456, #18040 ) ;
#17322 = CARTESIAN_POINT ( 'NONE',  ( 10.70799354677379256, -35.16985127952393242, 2.800654218530485018 ) ) ;
#17323 = AXIS2_PLACEMENT_3D ( 'NONE', #2765, #1042, #16734 ) ;
#17324 = CIRCLE ( 'NONE', #1972, 31.50000000000000711 ) ;
#17326 = EDGE_CURVE ( 'NONE', #15060, #13151, #5248, .T. ) ;
#17325 = ORIENTED_EDGE ( 'NONE', *, *, #7936, .F. ) ;
#17327 = B_SPLINE_CURVE_WITH_KNOTS ( 'NONE', 3,
 ( #21242, #9321, #5647, #19641 ),
 .UNSPECIFIED., .F., .F.,
 ( 4, 4 ),
 ( 0.001875451646902835971, 0.003761979286331349620 ),
 .UNSPECIFIED. ) ;
#17328 = EDGE_CURVE ( 'NONE', #928, #12190, #9351, .T. ) ;
#17329 = ORIENTED_EDGE ( 'NONE', *, *, #14202, .F. ) ;
#17330 = EDGE_LOOP ( 'NONE', ( #9482, #14255, #19866, #10668 ) ) ;
#17331 = FACE_OUTER_BOUND ( 'NONE', #4741, .T. ) ;
#17332 = EDGE_LOOP ( 'NONE', ( #18765, #11334, #19055, #9898 ) ) ;
#17333 = CARTESIAN_POINT ( 'NONE',  ( 2.775557561562891351E-14, 2.775557561562891351E-14, 5.750000000000001776 ) ) ;
#17334 = CARTESIAN_POINT ( 'NONE',  ( 19.90501858586606332, 9.588439829449720619, 58.07150046051953041 ) ) ;
#17335 = AXIS2_PLACEMENT_3D ( 'NONE', #10713, #17608, #307 ) ;
#17336 = CYLINDRICAL_SURFACE ( 'NONE', #21267, 2.499999999999995115 ) ;
#17337 = CARTESIAN_POINT ( 'NONE',  ( 5.345263474800246328, 40.00000000000000711, 51.78208639683223424 ) ) ;
#17338 = ADVANCED_FACE ( 'NONE', ( #12712 ), #14658, .T. ) ;
#17339 = ORIENTED_EDGE ( 'NONE', *, *, #1382, .F. ) ;
#17340 = DIRECTION ( 'NONE',  ( 0.000000000000000000, 0.000000000000000000, 1.000000000000000000 ) ) ;
#17341 = CARTESIAN_POINT ( 'NONE',  ( -5.833333333333327708, 6.180730040185831164, 40.61164310337068173 ) ) ;
#17342 = ORIENTED_EDGE ( 'NONE', *, *, #14281, .F. ) ;
#17343 = VECTOR ( 'NONE', #16465, 1000.000000000000000 ) ;
#17344 = ORIENTED_EDGE ( 'NONE', *, *, #16592, .T. ) ;
#17345 = FACE_OUTER_BOUND ( 'NONE', #11265, .T. ) ;
#17346 = VERTEX_POINT ( 'NONE', #18223 ) ;
#17347 = CARTESIAN_POINT ( 'NONE',  ( -6.070730550690822902, -31.88709182564697286, -7.000000000000006217 ) ) ;
#17348 = CARTESIAN_POINT ( 'NONE',  ( 35.00000000000001421, 0.000000000000000000, 1.540743955509788682E-30 ) ) ;
#17349 = CARTESIAN_POINT ( 'NONE',  ( -1.080479714573465255, 39.99305457876869951, 49.55623352467100773 ) ) ;
#17350 = PRESENTATION_LAYER_ASSIGNMENT (  '', '', ( #15508 ) ) ;
#17351 = CARTESIAN_POINT ( 'NONE',  ( 16.71858216490069893, 8.984148545337202307, 57.18548413420058552 ) ) ;
#17352 = CARTESIAN_POINT ( 'NONE',  ( 7.980461308159936706, -36.39375341857525825, 3.000000000000023537 ) ) ;
#17353 = CARTESIAN_POINT ( 'NONE',  ( 12.99999999999993960, 42.51666049839543149, 105.0000000000000142 ) ) ;
#17354 = CIRCLE ( 'NONE', #9314, 8.999999999999998224 ) ;
#17355 = EDGE_LOOP ( 'NONE', ( #19553, #14154, #8522, #5715 ) ) ;
#17356 = ORIENTED_EDGE ( 'NONE', *, *, #12158, .T. ) ;
#17357 = ORIENTED_EDGE ( 'NONE', *, *, #21284, .F. ) ;
#17358 = CIRCLE ( 'NONE', #533, 3.399999999999995470 ) ;
#17359 = ORIENTED_EDGE ( 'NONE', *, *, #12635, .T. ) ;
#17360 = DIRECTION ( 'NONE',  ( 0.000000000000000000, 0.000000000000000000, 1.000000000000000000 ) ) ;
#17361 = DIRECTION ( 'NONE',  ( -0.1421319796954317316, 0.000000000000000000, -0.9898477157360406897 ) ) ;
#17362 = CARTESIAN_POINT ( 'NONE',  ( 35.00000000000000000, 22.00000000000000355, 2.365113165210053967E-14 ) ) ;
#17363 = CARTESIAN_POINT ( 'NONE',  ( 0.6551139140931220295, 39.99751804686117396, 49.23721919104350775 ) ) ;
#17364 = ORIENTED_EDGE ( 'NONE', *, *, #1264, .F. ) ;
#17365 = CARTESIAN_POINT ( 'NONE',  ( -33.52953626616041305, -9.708269511265326557, -2.999999999999971578 ) ) ;
#17366 = CARTESIAN_POINT ( 'NONE',  ( -5.967611715581248255, 40.00000000000000711, -52.07955728799370831 ) ) ;
#17367 = DIRECTION ( 'NONE',  ( -0.000000000000000000, -0.000000000000000000, 1.000000000000000000 ) ) ;
#17368 = CYLINDRICAL_SURFACE ( 'NONE', #2419, 2.500000000000008882 ) ;
#17369 = DIRECTION ( 'NONE',  ( -1.000000000000000000, 0.000000000000000000, 0.000000000000000000 ) ) ;
#17370 = EDGE_CURVE ( 'NONE', #3635, #7032, #9172, .T. ) ;
#17371 = CIRCLE ( 'NONE', #4205, 19.11328065563150957 ) ;
#17372 = EDGE_LOOP ( 'NONE', ( #12700, #460 ) ) ;
#17373 = CARTESIAN_POINT ( 'NONE',  ( 31.67162468656012209, 14.67611967928900185, 3.000000000000002665 ) ) ;
#17374 = EDGE_CURVE ( 'NONE', #8029, #19756, #934, .T. ) ;
#17375 = ORIENTED_EDGE ( 'NONE', *, *, #7753, .F. ) ;
#17376 = EDGE_CURVE ( 'NONE', #15616, #12921, #12607, .T. ) ;
#17377 = CYLINDRICAL_SURFACE ( 'NONE', #8557, 49.99999999999998579 ) ;
#17378 = CARTESIAN_POINT ( 'NONE',  ( -1.387778780781445518E-14, 20.00000000000000355, -102.0000000000000142 ) ) ;
#17379 = DIRECTION ( 'NONE',  ( -1.000000000000000000, 0.000000000000000000, 0.000000000000000000 ) ) ;
#17380 = ORIENTED_EDGE ( 'NONE', *, *, #6689, .F. ) ;
#17381 = ORIENTED_EDGE ( 'NONE', *, *, #22220, .T. ) ;
#17382 = EDGE_LOOP ( 'NONE', ( #21953, #14073, #17879, #7236 ) ) ;
#17383 = AXIS2_PLACEMENT_3D ( 'NONE', #5401, #12382, #15809 ) ;
#17384 = DIRECTION ( 'NONE',  ( 0.000000000000000000, 0.000000000000000000, 1.000000000000000000 ) ) ;
#17385 = EDGE_CURVE ( 'NONE', #10749, #19781, #4251, .T. ) ;
#17386 = CARTESIAN_POINT ( 'NONE',  ( -24.79619811426202247, 21.00948735876864859, 3.000000000000023537 ) ) ;
#17387 = ORIENTED_EDGE ( 'NONE', *, *, #5660, .F. ) ;
#17388 = DIRECTION ( 'NONE',  ( 6.505213034913038160E-19, 3.903127820947822896E-18, 1.000000000000000000 ) ) ;
#17389 = CARTESIAN_POINT ( 'NONE',  ( -42.50000000000000711, -5.000000000000000000, 49.60000000000000853 ) ) ;
#17390 = CARTESIAN_POINT ( 'NONE',  ( 90.00000000000000000, 28.00000000000000000, -2.099999999999991651 ) ) ;
#17391 = AXIS2_PLACEMENT_3D ( 'NONE', #3254, #17211, #1526 ) ;
#17392 = EDGE_CURVE ( 'NONE', #8509, #10027, #14822, .T. ) ;
#17393 = CARTESIAN_POINT ( 'NONE',  ( -18.14075711706056993, 28.59859666634928743, -57.62969612438654110 ) ) ;
#17394 = DIRECTION ( 'NONE',  ( -0.000000000000000000, -1.000000000000000000, -0.000000000000000000 ) ) ;
#17395 = AXIS2_PLACEMENT_3D ( 'NONE', #22411, #6703, #20683 ) ;
#17396 = ORIENTED_EDGE ( 'NONE', *, *, #11335, .T. ) ;
#17397 = CYLINDRICAL_SURFACE ( 'NONE', #5018, 36.76383501243555685 ) ;
#17398 = CARTESIAN_POINT ( 'NONE',  ( 17.00000000000000000, 20.00000000000000711, -102.0000000000000142 ) ) ;
#17399 = AXIS2_PLACEMENT_3D ( 'NONE', #14177, #15564, #10522 ) ;
#17400 = CARTESIAN_POINT ( 'NONE',  ( -7.505578006075205089, 1.461761173328240515, 55.63523492904089096 ) ) ;
#17401 = DIRECTION ( 'NONE',  ( -1.445602896647339410E-16, -0.000000000000000000, -1.000000000000000000 ) ) ;
#17402 = EDGE_CURVE ( 'NONE', #2694, #66, #557, .T. ) ;
#17403 = AXIS2_PLACEMENT_3D ( 'NONE', #3529, #14025, #7061 ) ;
#17404 = ORIENTED_EDGE ( 'NONE', *, *, #15974, .F. ) ;
#17405 = LINE ( 'NONE', #10628, #14091 ) ;
#17406 = CARTESIAN_POINT ( 'NONE',  ( -34.99999999999997868, -5.000000000000000000, 54.99999999999698730 ) ) ;
#17407 = VERTEX_POINT ( 'NONE', #7454 ) ;
#17408 = EDGE_CURVE ( 'NONE', #14094, #2582, #19733, .T. ) ;
#17409 = APPLICATION_PROTOCOL_DEFINITION ( 'draft international standard', 'automotive_design', 1998, #11506 ) ;
#17410 = ORIENTED_EDGE ( 'NONE', *, *, #3860, .T. ) ;
#17411 = CARTESIAN_POINT ( 'NONE',  ( 7.310544252644470693E-15, 28.19616000222403684, 0.000000000000000000 ) ) ;
#17412 = CIRCLE ( 'NONE', #13381, 2.500000000000002220 ) ;
#17413 = CARTESIAN_POINT ( 'NONE',  ( 35.51751788033374879, -1.011722470948249963, -2.999999999999986677 ) ) ;
#17414 = DIRECTION ( 'NONE',  ( 0.000000000000000000, 0.000000000000000000, 1.000000000000000000 ) ) ;
#17415 = DIRECTION ( 'NONE',  ( 0.000000000000000000, 0.5150380749100562650, 0.8571673007021111124 ) ) ;
#17416 = DIRECTION ( 'NONE',  ( 0.000000000000000000, 1.000000000000000000, -0.000000000000000000 ) ) ;
#17417 = ORIENTED_EDGE ( 'NONE', *, *, #9809, .F. ) ;
#17418 = DIRECTION ( 'NONE',  ( 0.000000000000000000, -0.7071067811865352493, -0.7071067811865597852 ) ) ;
#17419 = CARTESIAN_POINT ( 'NONE',  ( 3.330669073875469621E-13, -1.110223024625156540E-13, -2.999999999999971578 ) ) ;
#17420 = ORIENTED_EDGE ( 'NONE', *, *, #21612, .F. ) ;
#17421 = ADVANCED_FACE ( 'NONE', ( #21557 ), #21779, .T. ) ;
#17423 = ADVANCED_FACE ( 'NONE', ( #13040 ), #5264, .T. ) ;
#17422 = CARTESIAN_POINT ( 'NONE',  ( 35.00000000000000000, 38.99999999999999289, 4.258610482196280173E-15 ) ) ;
#17424 = CARTESIAN_POINT ( 'NONE',  ( 21.07599011712227011, 12.09199673218656024, -58.36745205258138469 ) ) ;
#17425 = LINE ( 'NONE', #8728, #10049 ) ;
#17426 = CARTESIAN_POINT ( 'NONE',  ( -3.999999999999993339, 28.19616000222403684, 0.000000000000000000 ) ) ;
#17427 = CARTESIAN_POINT ( 'NONE',  ( -3.019669046279628510, 39.94555832068629542, -50.93804386297323106 ) ) ;
#17428 = EDGE_LOOP ( 'NONE', ( #18271, #12047 ) ) ;
#17429 = CARTESIAN_POINT ( 'NONE',  ( -30.60042966911713336, -7.474202570536353285, -6.999999999999992006 ) ) ;
#17430 = CARTESIAN_POINT ( 'NONE',  ( -20.15166188517206791, 29.89072699358926499, 58.13409936646347376 ) ) ;
#17431 = VECTOR ( 'NONE', #6571, 1000.000000000000000 ) ;
#17432 = ORIENTED_EDGE ( 'NONE', *, *, #12013, .F. ) ;
#17433 = FACE_OUTER_BOUND ( 'NONE', #16221, .T. ) ;
#17434 = DIRECTION ( 'NONE',  ( 0.000000000000000000, 0.7071067811865500152, -0.7071067811865451302 ) ) ;
#17435 = ADVANCED_FACE ( 'NONE', ( #1143 ), #2026, .F. ) ;
#17436 = LINE ( 'NONE', #10106, #10710 ) ;
#17437 = CIRCLE ( 'NONE', #6476, 31.50000000000000711 ) ;
#17438 = EDGE_CURVE ( 'NONE', #19421, #13519, #6533, .T. ) ;
#17439 = ORIENTED_EDGE ( 'NONE', *, *, #18959, .F. ) ;
#17440 = ORIENTED_EDGE ( 'NONE', *, *, #20711, .T. ) ;
#17441 = EDGE_CURVE ( 'NONE', #6416, #22614, #2758, .T. ) ;
#17442 = ORIENTED_EDGE ( 'NONE', *, *, #7634, .F. ) ;
#17443 = SHAPE_REPRESENTATION_RELATIONSHIP ( 'NONE' , 'NONE' ,  #6502, #7164 ) ;
#17444 = CIRCLE ( 'NONE', #12313, 2.099999999999997868 ) ;
#17445 = ORIENTED_EDGE ( 'NONE', *, *, #14778, .T. ) ;
#17446 = DIRECTION ( 'NONE',  ( 0.000000000000000000, -1.000000000000000000, 0.000000000000000000 ) ) ;
#17447 = CARTESIAN_POINT ( 'NONE',  ( 16.62266455332486714, 35.11598757108757951, 57.12012504743141506 ) ) ;
#17448 = DIRECTION ( 'NONE',  ( 0.000000000000000000, -0.000000000000000000, 1.000000000000000000 ) ) ;
#17449 = CARTESIAN_POINT ( 'NONE',  ( 8.448970453231776645, 40.00000000000000000, 53.13698759631014923 ) ) ;
#17450 = ORIENTED_EDGE ( 'NONE', *, *, #10505, .T. ) ;
#17451 = CARTESIAN_POINT ( 'NONE',  ( 3.071904583821672593E-15, -4.500000000000010658, 0.000000000000000000 ) ) ;
#17452 = CARTESIAN_POINT ( 'NONE',  ( -4.078319513017746090, 5.557204472854577304, 39.58919430873140755 ) ) ;
#17453 = ORIENTED_EDGE ( 'NONE', *, *, #14623, .F. ) ;
#17454 = DIRECTION ( 'NONE',  ( 6.505213034913038160E-19, 3.903127820947822896E-18, 1.000000000000000000 ) ) ;
#17455 = CARTESIAN_POINT ( 'NONE',  ( 21.94460005644907596, 28.73837443790550239, -2.932164912090539310 ) ) ;
#17456 = EDGE_LOOP ( 'NONE', ( #6440, #10575 ) ) ;
#17457 = DIRECTION ( 'NONE',  ( 1.266830946243004623E-16, -1.000000000000000000, -3.903127820947817503E-18 ) ) ;
#17458 = EDGE_LOOP ( 'NONE', ( #9398, #1703, #20814, #8657, #7007, #603 ) ) ;
#17459 = FACE_OUTER_BOUND ( 'NONE', #1707, .T. ) ;
#17460 = CARTESIAN_POINT ( 'NONE',  ( -5.302679949206207333, 39.28774282260670248, 54.25155191766013019 ) ) ;
#17461 = CARTESIAN_POINT ( 'NONE',  ( 36.75746821813321930, -0.6841746959067585010, -2.800654218530457484 ) ) ;
#17462 = EDGE_CURVE ( 'NONE', #14484, #21816, #11572, .T. ) ;
#17463 = AXIS2_PLACEMENT_3D ( 'NONE', #9091, #377, #16294 ) ;
#17464 = CIRCLE ( 'NONE', #5753, 12.00000000000000000 ) ;
#17465 = CARTESIAN_POINT ( 'NONE',  ( 22.05221796475640161, 24.18157222985895061, 58.58672997743932598 ) ) ;
#17466 = DIRECTION ( 'NONE',  ( 0.000000000000000000, 1.000000000000000000, 0.000000000000000000 ) ) ;
#17467 = AXIS2_PLACEMENT_3D ( 'NONE', #13831, #4806, #11775 ) ;
#17468 = CARTESIAN_POINT ( 'NONE',  ( -17.32050807568840867, -1.500000000000011768, -10.00000000000061284 ) ) ;
#17469 = ADVANCED_FACE ( 'NONE', ( #5044 ), #9738, .F. ) ;
#17470 = B_SPLINE_CURVE_WITH_KNOTS ( 'NONE', 3,
 ( #13865, #8725, #8494, #3466, #20879, #10424, #20986, #17543, #15468, #5183 ),
 .UNSPECIFIED., .F., .F.,
 ( 4, 2, 2, 2, 4 ),
 ( 1.181610135877042463E-17, 0.002975785561748149188, 0.005951571123496287100, 0.008927356685244424578, 0.01190314224699256206 ),
 .UNSPECIFIED. ) ;
#17471 = ORIENTED_EDGE ( 'NONE', *, *, #190, .F. ) ;
#17472 = ORIENTED_EDGE ( 'NONE', *, *, #4345, .T. ) ;
#17473 = VECTOR ( 'NONE', #9004, 1000.000000000000000 ) ;
#17474 = ORIENTED_EDGE ( 'NONE', *, *, #11126, .F. ) ;
#17475 = ORIENTED_EDGE ( 'NONE', *, *, #10054, .T. ) ;
#17476 = DIRECTION ( 'NONE',  ( 0.000000000000000000, 0.000000000000000000, -1.000000000000000000 ) ) ;
#17477 = DIRECTION ( 'NONE',  ( 0.000000000000000000, 0.000000000000000000, -1.000000000000000000 ) ) ;
#17478 = AXIS2_PLACEMENT_3D ( 'NONE', #13157, #2532, #4706 ) ;
#17479 = CIRCLE ( 'NONE', #7610, 0.9999999999999974465 ) ;
#17480 = DIRECTION ( 'NONE',  ( -0.000000000000000000, -1.000000000000000000, -0.000000000000000000 ) ) ;
#17481 = CARTESIAN_POINT ( 'NONE',  ( 19.99999999999999645, -4.500000000000013323, 0.000000000000000000 ) ) ;
#17482 = CARTESIAN_POINT ( 'NONE',  ( 0.05877019086828588756, 39.99997968727448949, 48.77966970436191474 ) ) ;
#17483 = CIRCLE ( 'NONE', #276, 10.00000000000000178 ) ;
#17484 = ORIENTED_EDGE ( 'NONE', *, *, #18258, .F. ) ;
#17485 = CARTESIAN_POINT ( 'NONE',  ( 42.49999999999998579, 10.00000000000000000, -47.49999999999997868 ) ) ;
#17486 = DIRECTION ( 'NONE',  ( 0.000000000000000000, 1.000000000000000000, 0.000000000000000000 ) ) ;
#17487 = DIRECTION ( 'NONE',  ( 0.7752116086454784449, 0.5577761202038514776, -0.2965345874457622211 ) ) ;
#17488 = FACE_OUTER_BOUND ( 'NONE', #13768, .T. ) ;
#17489 = SURFACE_SIDE_STYLE ('',( #15415 ) ) ;
#17490 = EDGE_CURVE ( 'NONE', #17574, #5266, #11782, .T. ) ;
#17491 = ORIENTED_EDGE ( 'NONE', *, *, #20473, .T. ) ;
#17492 = VECTOR ( 'NONE', #19711, 1000.000000000000114 ) ;
#17493 = CARTESIAN_POINT ( 'NONE',  ( -19.62614308895802750, 23.87978888144413858, 60.53224704373671727 ) ) ;
#17494 = AXIS2_PLACEMENT_3D ( 'NONE', #16293, #11135, #15946 ) ;
#17495 = AXIS2_PLACEMENT_3D ( 'NONE', #16698, #15071, #13349 ) ;
#17496 = CARTESIAN_POINT ( 'NONE',  ( -8.957612896613865061, 39.56965375125236051, 54.21301076066360736 ) ) ;
#17497 = EDGE_CURVE ( 'NONE', #11475, #13563, #22119, .T. ) ;
#17498 = DIRECTION ( 'NONE',  ( 0.000000000000000000, 1.000000000000000000, 0.000000000000000000 ) ) ;
#17499 = AXIS2_PLACEMENT_3D ( 'NONE', #17603, #17711, #5464 ) ;
#17500 = LINE ( 'NONE', #14500, #10108 ) ;
#17501 = VECTOR ( 'NONE', #18130, 1000.000000000000000 ) ;
#17502 = ORIENTED_EDGE ( 'NONE', *, *, #12414, .T. ) ;
#17503 = ORIENTED_EDGE ( 'NONE', *, *, #785, .F. ) ;
#17504 = EDGE_CURVE ( 'NONE', #16050, #6428, #13340, .T. ) ;
#17505 = VERTEX_POINT ( 'NONE', #1483 ) ;
#17506 = CARTESIAN_POINT ( 'NONE',  ( 90.00000000000000000, 39.97500000000000142, -9.108981535246192915E-16 ) ) ;
#17507 = CIRCLE ( 'NONE', #10543, 9.000000000000003553 ) ;
#17508 = CARTESIAN_POINT ( 'NONE',  ( -31.67162468655987340, -14.67611967928944594, -2.999999999999971578 ) ) ;
#17509 = ORIENTED_EDGE ( 'NONE', *, *, #3282, .T. ) ;
#17510 = VECTOR ( 'NONE', #10258, 1000.000000000000000 ) ;
#17511 = EDGE_CURVE ( 'NONE', #1471, #22647, #4591, .T. ) ;
#17512 = DIRECTION ( 'NONE',  ( -6.505213034913038160E-19, -3.903127820947822896E-18, -1.000000000000000000 ) ) ;
#17513 = CARTESIAN_POINT ( 'NONE',  ( 25.34312177887357365, -20.17230487860815913, -2.999999999999999112 ) ) ;
#17514 = CARTESIAN_POINT ( 'NONE',  ( 17.66631876130919565, -31.41173278719250206, -2.999999999999999112 ) ) ;
#17515 = CARTESIAN_POINT ( 'NONE',  ( -9.998533603140344894, 40.00000000000000000, -54.54288842742649734 ) ) ;
#17516 = AXIS2_PLACEMENT_3D ( 'NONE', #5393, #2064, #3790 ) ;
#17517 = FACE_BOUND ( 'NONE', #2892, .T. ) ;
#17518 = PRODUCT ( 'REAR COVER', 'REAR COVER', '', ( #1727 ) ) ;
#17519 = ORIENTED_EDGE ( 'NONE', *, *, #3324, .F. ) ;
#17520 = DIRECTION ( 'NONE',  ( 0.000000000000000000, 0.000000000000000000, -1.000000000000000000 ) ) ;
#17521 = FACE_OUTER_BOUND ( 'NONE', #2095, .T. ) ;
#17522 = CYLINDRICAL_SURFACE ( 'NONE', #19261, 2.099999999999990763 ) ;
#17523 = DIRECTION ( 'NONE',  ( -1.000000000000000000, 0.000000000000000000, 0.000000000000000000 ) ) ;
#17524 = ORIENTED_EDGE ( 'NONE', *, *, #1644, .T. ) ;
#17525 = CIRCLE ( 'NONE', #3641, 4.000000000000000000 ) ;
#17526 = B_SPLINE_CURVE_WITH_KNOTS ( 'NONE', 3,
 ( #9222, #9461, #14601, #12767, #14480, #5791, #19881, #9118, #3969, #7393, #10939, #4082, #19777 ),
 .UNSPECIFIED., .F., .F.,
 ( 4, 2, 1, 1, 1, 2, 2, 4 ),
 ( 0.000000000000000000, 0.2499999999999938383, 0.3749999999999902300, 0.4374999999999883982, 0.4687499999999868439, 0.4843749999999850675, 0.4999999999999832911, 1.000000000000000000 ),
 .UNSPECIFIED. ) ;
#17527 = CARTESIAN_POINT ( 'NONE',  ( 26.79308242454919764, 16.56444186175085065, 2.999999999999995559 ) ) ;
#17528 = DIRECTION ( 'NONE',  ( 0.000000000000000000, 0.000000000000000000, 1.000000000000000000 ) ) ;
#17529 = AXIS2_PLACEMENT_3D ( 'NONE', #11252, #20313, #4501 ) ;
#17530 = PRODUCT_DEFINITION_FORMATION_WITH_SPECIFIED_SOURCE ( 'ANY', '', #8039, .NOT_KNOWN. ) ;
#17531 = ORIENTED_EDGE ( 'NONE', *, *, #7174, .T. ) ;
#17532 = EDGE_LOOP ( 'NONE', ( #2934, #14359, #21217 ) ) ;
#17533 = DIRECTION ( 'NONE',  ( -0.000000000000000000, 1.000000000000000000, -0.000000000000000000 ) ) ;
#17534 = EDGE_CURVE ( 'NONE', #10705, #17179, #11003, .T. ) ;
#17535 = DIRECTION ( 'NONE',  ( -0.000000000000000000, 1.000000000000000000, -0.000000000000000000 ) ) ;
#17536 = CARTESIAN_POINT ( 'NONE',  ( -34.99999999999998579, -5.000000000000000000, -59.99999999999703704 ) ) ;
#17537 = CIRCLE ( 'NONE', #4383, 2.500000000000008882 ) ;
#17538 = FACE_OUTER_BOUND ( 'NONE', #13881, .T. ) ;
#17539 = ORIENTED_EDGE ( 'NONE', *, *, #9991, .T. ) ;
#17540 = CARTESIAN_POINT ( 'NONE',  ( 2.220446049250313081E-13, -8.326672684688674053E-14, 2.800654218530498785 ) ) ;
#17541 = LINE ( 'NONE', #20641, #10157 ) ;
#17542 = ORIENTED_EDGE ( 'NONE', *, *, #18574, .T. ) ;
#17543 = CARTESIAN_POINT ( 'NONE',  ( 8.479740367039916293, -4.901256658985767345, -50.57596245086818243 ) ) ;
#17544 = CARTESIAN_POINT ( 'NONE',  ( 14.68518659845079100, 36.96998281527655195, -56.45735093204005040 ) ) ;
#17545 = CARTESIAN_POINT ( 'NONE',  ( 3.608224830031758756E-13, -2.775557561562891351E-14, -4.999999999999997335 ) ) ;
#17546 = CARTESIAN_POINT ( 'NONE',  ( -9.728382627765713053, 39.99999999999997868, -53.57939893134117426 ) ) ;
#17547 = ORIENTED_EDGE ( 'NONE', *, *, #3436, .T. ) ;
#17548 = CARTESIAN_POINT ( 'NONE',  ( -9.952189117650803496, 40.00000000000000000, 53.64426396172073908 ) ) ;
#17549 = CARTESIAN_POINT ( 'NONE',  ( -22.15746142094444338, 16.52917608750725975, 58.60949679988863892 ) ) ;
#17550 = VERTEX_POINT ( 'NONE', #16010 ) ;
#17551 = DIRECTION ( 'NONE',  ( 6.505213034913038160E-19, 3.903127820947822896E-18, 1.000000000000000000 ) ) ;
#17552 = ADVANCED_FACE ( 'NONE', ( #14165 ), #18867, .T. ) ;
#17553 = DIRECTION ( 'NONE',  ( 0.000000000000000000, 0.000000000000000000, -1.000000000000000000 ) ) ;
#17554 = DIRECTION ( 'NONE',  ( 0.000000000000000000, 0.000000000000000000, -1.000000000000000000 ) ) ;
#17555 = CIRCLE ( 'NONE', #15345, 14.00000000000000000 ) ;
#17556 = ADVANCED_FACE ( 'NONE', ( #15890, #21070 ), #5160, .T. ) ;
#17557 = ORIENTED_EDGE ( 'NONE', *, *, #4622, .T. ) ;
#17558 = VERTEX_POINT ( 'NONE', #10511 ) ;
#17559 = ORIENTED_EDGE ( 'NONE', *, *, #15974, .T. ) ;
#17560 =( LENGTH_UNIT ( ) NAMED_UNIT ( * ) SI_UNIT ( .MILLI., .METRE. ) );
#17561 = VERTEX_POINT ( 'NONE', #10572 ) ;
#17562 = LINE ( 'NONE', #15721, #12174 ) ;
#17563 = CARTESIAN_POINT ( 'NONE',  ( 19.47136665037375636, 8.793048248091398733, 57.95785196855348431 ) ) ;
#17564 = CIRCLE ( 'NONE', #6225, 2.499999999999995115 ) ;
#17565 = FACE_OUTER_BOUND ( 'NONE', #16619, .T. ) ;
#17566 = DIRECTION ( 'NONE',  ( -6.505213034913038160E-19, -3.903127820947822896E-18, -1.000000000000000000 ) ) ;
#17567 = ORIENTED_EDGE ( 'NONE', *, *, #4066, .F. ) ;
#17568 = DIRECTION ( 'NONE',  ( -0.000000000000000000, 1.000000000000000000, -0.000000000000000000 ) ) ;
#17569 = CARTESIAN_POINT ( 'NONE',  ( -4.986731981817630555, 5.845158537422243228, 40.05110651909059527 ) ) ;
#17570 = ORIENTED_EDGE ( 'NONE', *, *, #650, .T. ) ;
#17571 = CARTESIAN_POINT ( 'NONE',  ( -4.663248442268214333, 0.4972264943030605400, 53.80945059829245736 ) ) ;
#17572 = CARTESIAN_POINT ( 'NONE',  ( -14.71244060472248272, 36.96434927850638985, -56.47085971327719989 ) ) ;
#17573 = FACE_OUTER_BOUND ( 'NONE', #12003, .T. ) ;
#17574 = VERTEX_POINT ( 'NONE', #12454 ) ;
#17575 = AXIS2_PLACEMENT_3D ( 'NONE', #602, #723, #18247 ) ;
#17576 = FACE_OUTER_BOUND ( 'NONE', #20222, .T. ) ;
#17577 = ORIENTED_EDGE ( 'NONE', *, *, #12349, .T. ) ;
#17578 = CARTESIAN_POINT ( 'NONE',  ( 2.775557561562891351E-14, 2.775557561562891351E-14, 5.750000000000001776 ) ) ;
#17579 = DIRECTION ( 'NONE',  ( -0.000000000000000000, -1.000000000000000000, -0.000000000000000000 ) ) ;
#17580 = CARTESIAN_POINT ( 'NONE',  ( -0.6620359884758859614, 39.99747031435470745, 49.24247971419962511 ) ) ;
#17581 = EDGE_CURVE ( 'NONE', #13828, #9986, #18118, .T. ) ;
#17582 = CARTESIAN_POINT ( 'NONE',  ( 21.16618710811372139, 27.45243199383212840, 58.38369730662807910 ) ) ;
#17583 = DIRECTION ( 'NONE',  ( 6.505213034913038160E-19, 3.903127820947822896E-18, 1.000000000000000000 ) ) ;
#17584 = AXIS2_PLACEMENT_3D ( 'NONE', #7907, #22002, #6295 ) ;
#17585 = CARTESIAN_POINT ( 'NONE',  ( 35.00000000000000000, 40.00000000000000000, 51.00000000000002842 ) ) ;
#17586 = ADVANCED_FACE ( 'NONE', ( #1713 ), #21296, .F. ) ;
#17587 = EDGE_CURVE ( 'NONE', #14484, #7482, #19128, .T. ) ;
#17589 = EDGE_CURVE ( 'NONE', #5664, #22237, #8597, .T. ) ;
#17588 = EDGE_LOOP ( 'NONE', ( #3456, #10344, #3308, #19971, #10228, #2527, #5669, #8260, #18722 ) ) ;
#17590 = ORIENTED_EDGE ( 'NONE', *, *, #22688, .F. ) ;
#17591 = ORIENTED_EDGE ( 'NONE', *, *, #612, .F. ) ;
#17592 = DIRECTION ( 'NONE',  ( -1.000000000000000000, 1.275531967630005245E-16, 0.000000000000000000 ) ) ;
#17593 = DIRECTION ( 'NONE',  ( -6.505213034913038160E-19, -3.903127820947822896E-18, -1.000000000000000000 ) ) ;
#17594 = EDGE_CURVE ( 'NONE', #17759, #9422, #19230, .T. ) ;
#17595 = CARTESIAN_POINT ( 'NONE',  ( 16.66666666666669272, -20.00000000000000000, -23.57022603955159212 ) ) ;
#17596 = AXIS2_PLACEMENT_3D ( 'NONE', #16205, #14486, #2133 ) ;
#17597 = DIRECTION ( 'NONE',  ( -0.000000000000000000, -0.000000000000000000, 1.000000000000000000 ) ) ;
#17598 = CARTESIAN_POINT ( 'NONE',  ( 1.321838024766639252, 39.98984255672822741, 49.73540085867594485 ) ) ;
#17599 = VECTOR ( 'NONE', #2318, 1000.000000000000000 ) ;
#17600 = VERTEX_POINT ( 'NONE', #1591 ) ;
#17601 = DIRECTION ( 'NONE',  ( -6.505213034913038160E-19, -3.903127820947822896E-18, -1.000000000000000000 ) ) ;
#17602 = DIRECTION ( 'NONE',  ( 0.000000000000000000, 0.000000000000000000, 1.000000000000000000 ) ) ;
#17603 = CARTESIAN_POINT ( 'NONE',  ( -42.50000000000000711, -12.00000000000000000, 47.50000000000000711 ) ) ;
#17604 = DIRECTION ( 'NONE',  ( -6.505213034913038160E-19, -3.903127820947822896E-18, -1.000000000000000000 ) ) ;
#17605 = CARTESIAN_POINT ( 'NONE',  ( 35.00000000000000000, -5.000000000000000000, 54.99999999999698019 ) ) ;
#17606 = LINE ( 'NONE', #1913, #10960 ) ;
#17607 = TOROIDAL_SURFACE ( 'NONE', #20551, 34.90673715956759082, 8.750000000000000000 ) ;
#17608 = DIRECTION ( 'NONE',  ( -0.000000000000000000, -0.000000000000000000, 1.000000000000000000 ) ) ;
#17609 = CARTESIAN_POINT ( 'NONE',  ( -2.347663744114242057, -31.41239365194214983, 2.999999999999995559 ) ) ;
#17610 = CARTESIAN_POINT ( 'NONE',  ( -24.73600648735115115, 27.19760187735867518, 2.800654218530485018 ) ) ;
#17611 = ORIENTED_EDGE ( 'NONE', *, *, #20260, .F. ) ;
#17612 = ORIENTED_EDGE ( 'NONE', *, *, #17003, .T. ) ;
#17613 = EDGE_CURVE ( 'NONE', #22196, #14743, #20856, .T. ) ;
#17614 = ORIENTED_EDGE ( 'NONE', *, *, #10719, .F. ) ;
#17615 = CARTESIAN_POINT ( 'NONE',  ( 8.460114887491986480, -4.900635315005658299, -50.56657553898721602 ) ) ;
#17616 = EDGE_CURVE ( 'NONE', #5838, #7355, #15781, .T. ) ;
#17617 = CARTESIAN_POINT ( 'NONE',  ( 11.73108507413468971, 40.00000000000000000, -54.23086838360208617 ) ) ;
#17618 = AXIS2_PLACEMENT_3D ( 'NONE', #600, #7362, #10904 ) ;
#17619 = CARTESIAN_POINT ( 'NONE',  ( 2.775557561562891351E-14, -2.775557561562891351E-14, 2.999999999999999112 ) ) ;
#17620 = ADVANCED_FACE ( 'NONE', ( #5373 ), #1829, .F. ) ;
#17621 = DIRECTION ( 'NONE',  ( 1.000000000000000000, 0.000000000000000000, 0.000000000000000000 ) ) ;
#17622 = CYLINDRICAL_SURFACE ( 'NONE', #15670, 30.00000000000000000 ) ;
#17623 = CARTESIAN_POINT ( 'NONE',  ( 30.48934413892814987, -16.99647590252656570, -2.999999999999971578 ) ) ;
#17624 = DIRECTION ( 'NONE',  ( 0.000000000000000000, -1.000000000000000000, 0.000000000000000000 ) ) ;
#17625 = VERTEX_POINT ( 'NONE', #3434 ) ;
#17626 = CARTESIAN_POINT ( 'NONE',  ( 35.00000000000000000, 22.00000000000000711, 2.255140518769849223E-14 ) ) ;
#17627 =( NAMED_UNIT ( * ) PLANE_ANGLE_UNIT ( ) SI_UNIT ( $, .RADIAN. ) );
#17628 = CARTESIAN_POINT ( 'NONE',  ( -35.00000000000000000, -4.928932188134504955, 57.07106781186553235 ) ) ;
#17629 = DIRECTION ( 'NONE',  ( -1.000000000000000000, 0.000000000000000000, -0.000000000000000000 ) ) ;
#17630 = CARTESIAN_POINT ( 'NONE',  ( 14.99999999999998579, 20.00000000000000355, -45.82575694955836809 ) ) ;
#17631 = ORIENTED_EDGE ( 'NONE', *, *, #16143, .F. ) ;
#17632 = CARTESIAN_POINT ( 'NONE',  ( -24.41514043009185286, -26.50842683089776841, -2.999999999999971578 ) ) ;
#17633 = CARTESIAN_POINT ( 'NONE',  ( 31.41173278719253048, 17.66631876130919565, -2.999999999999971578 ) ) ;
#17634 = EDGE_CURVE ( 'NONE', #2582, #15060, #4966, .T. ) ;
#17635 = AXIS2_PLACEMENT_3D ( 'NONE', #9740, #9954, #15216 ) ;
#17636 = ORIENTED_EDGE ( 'NONE', *, *, #2744, .T. ) ;
#17637 = ORIENTED_EDGE ( 'NONE', *, *, #20667, .T. ) ;
#17638 = DIRECTION ( 'NONE',  ( 0.000000000000000000, 0.000000000000000000, 1.000000000000000000 ) ) ;
#17639 = DIRECTION ( 'NONE',  ( 0.000000000000000000, 0.000000000000000000, -1.000000000000000000 ) ) ;
#17640 = CARTESIAN_POINT ( 'NONE',  ( -8.916870955515566521, 2.080241304161454252, 56.50845996868352472 ) ) ;
#17641 = DIRECTION ( 'NONE',  ( 0.000000000000000000, 0.000000000000000000, 1.000000000000000000 ) ) ;
#17642 = ORIENTED_EDGE ( 'NONE', *, *, #17497, .F. ) ;
#17643 = DIRECTION ( 'NONE',  ( -0.000000000000000000, -1.000000000000000000, -0.000000000000000000 ) ) ;
#17644 = CARTESIAN_POINT ( 'NONE',  ( -9.038714882927470384, 40.00000000000001421, 53.35170948314333117 ) ) ;
#17645 = ORIENTED_EDGE ( 'NONE', *, *, #15691, .T. ) ;
#17646 = CARTESIAN_POINT ( 'NONE',  ( -31.67162468655980589, -14.67611967928950101, 3.000000000000002665 ) ) ;
#17647 = CARTESIAN_POINT ( 'NONE',  ( 17.98964431006456977, 6.536084871031931698, -57.54127157382310287 ) ) ;
#17648 = AXIS2_PLACEMENT_3D ( 'NONE', #4081, #11048, #21148 ) ;
#17649 = CARTESIAN_POINT ( 'NONE',  ( 4.177897941877526833, -34.13396246814587442, 3.000000000000023537 ) ) ;
#17650 = CARTESIAN_POINT ( 'NONE',  ( 31.88709182564702971, -6.070730550690850436, -6.999999999999999112 ) ) ;
#17651 = EDGE_LOOP ( 'NONE', ( #9187, #16980, #18470, #4831, #10446, #17939, #13530 ) ) ;
#17652 = CARTESIAN_POINT ( 'NONE',  ( -34.99999999999999289, -5.000000000000000000, -3.012171160963566127E-14 ) ) ;
#17653 = CARTESIAN_POINT ( 'NONE',  ( -9.103081159019538404, 0.03030367950604238858, 53.87333532811888404 ) ) ;
#17654 = CARTESIAN_POINT ( 'NONE',  ( 0.000000000000000000, 15.00000000000000000, 0.000000000000000000 ) ) ;
#17655 = EDGE_CURVE ( 'NONE', #8747, #15126, #12240, .T. ) ;
#17656 = ORIENTED_EDGE ( 'NONE', *, *, #6421, .T. ) ;
#17657 = CARTESIAN_POINT ( 'NONE',  ( 35.00000000000000000, 25.00000000000000000, 2.365113165210053967E-14 ) ) ;
#17658 = DIRECTION ( 'NONE',  ( 0.000000000000000000, 0.000000000000000000, 1.000000000000000000 ) ) ;
#17659 = ADVANCED_FACE ( 'NONE', ( #7195, #17517, #12351 ), #10619, .T. ) ;
#17660 = EDGE_CURVE ( 'NONE', #18225, #349, #11899, .T. ) ;
#17661 = ORIENTED_EDGE ( 'NONE', *, *, #19291, .F. ) ;
#17662 = ORIENTED_EDGE ( 'NONE', *, *, #6094, .T. ) ;
#17663 = ORIENTED_EDGE ( 'NONE', *, *, #6617, .F. ) ;
#17664 =( LENGTH_UNIT ( ) NAMED_UNIT ( * ) SI_UNIT ( .MILLI., .METRE. ) );
#17665 = AXIS2_PLACEMENT_3D ( 'NONE', #9993, #4964, #12279 ) ;
#17666 = ORIENTED_EDGE ( 'NONE', *, *, #2745, .F. ) ;
#17667 = DIRECTION ( 'NONE',  ( 6.505213034913038160E-19, 3.903127820947822896E-18, 1.000000000000000000 ) ) ;
#17668 = DIRECTION ( 'NONE',  ( -1.000000000000000000, -1.208970125616027129E-17, 0.000000000000000000 ) ) ;
#17669 = CARTESIAN_POINT ( 'NONE',  ( -48.93401015228426587, 10.00000000000000000, 46.57614213197968667 ) ) ;
#17670 = CARTESIAN_POINT ( 'NONE',  ( 4.719078569232699749, 39.99999999999999289, 51.46810808308088525 ) ) ;
#17671 = EDGE_CURVE ( 'NONE', #8384, #8973, #10774, .T. ) ;
#17672 = ORIENTED_EDGE ( 'NONE', *, *, #11678, .F. ) ;
#17673 = DIRECTION ( 'NONE',  ( -0.000000000000000000, -0.000000000000000000, -1.000000000000000000 ) ) ;
#17674 = CARTESIAN_POINT ( 'NONE',  ( -0.6683989176636820906, -3.155640224527792359, -47.80307817979882401 ) ) ;
#17675 = EDGE_LOOP ( 'NONE', ( #14157, #9756, #6692, #20578 ) ) ;
#17676 = DIRECTION ( 'NONE',  ( -1.000000000000000000, 0.000000000000000000, 0.000000000000000000 ) ) ;
#17677 = DIRECTION ( 'NONE',  ( -0.000000000000000000, 1.000000000000000000, -0.000000000000000000 ) ) ;
#17678 = DIRECTION ( 'NONE',  ( 1.000000000000000000, 0.000000000000000000, 0.000000000000000000 ) ) ;
#17679 = ORIENTED_EDGE ( 'NONE', *, *, #14436, .T. ) ;
#17680 = CARTESIAN_POINT ( 'NONE',  ( 6.002321937219792680, -0.8366808808196497527, 52.11647083208005427 ) ) ;
#17681 = ORIENTED_EDGE ( 'NONE', *, *, #21833, .F. ) ;
#17682 = CARTESIAN_POINT ( 'NONE',  ( 0.7060561200947481630, 40.00000000000296296, -49.41654807903094593 ) ) ;
#17683 = EDGE_CURVE ( 'NONE', #6172, #4131, #21750, .T. ) ;
#17684 = FACE_OUTER_BOUND ( 'NONE', #20925, .T. ) ;
#17685 = SURFACE_STYLE_USAGE ( .BOTH. , #9104 ) ;
#17686 = CARTESIAN_POINT ( 'NONE',  ( 34.13396246814617996, -14.93538271375438597, -6.999999999999950262 ) ) ;
#17687 = TOROIDAL_SURFACE ( 'NONE', #497, 18.00000000000000355, 4.000000000000000000 ) ;
#17688 = CARTESIAN_POINT ( 'NONE',  ( 19.94270148199750281, 21.57319560958842430, 58.13234078200308375 ) ) ;
#17689 = DIRECTION ( 'NONE',  ( 0.000000000000000000, 0.000000000000000000, 1.000000000000000000 ) ) ;
#17690 = CIRCLE ( 'NONE', #11107, 6.499999999999999112 ) ;
#17691 = TOROIDAL_SURFACE ( 'NONE', #7807, 34.90673715956759082, 8.750000000000000000 ) ;
#17692 = CARTESIAN_POINT ( 'NONE',  ( 28.73472116836727253, -21.94328778841628136, 2.932969818539057361 ) ) ;
#17693 = ORIENTED_EDGE ( 'NONE', *, *, #9588, .T. ) ;
#17694 = AXIS2_PLACEMENT_3D ( 'NONE', #22076, #15965, #8873 ) ;
#17695 = VERTEX_POINT ( 'NONE', #9380 ) ;
#17696 = ORIENTED_EDGE ( 'NONE', *, *, #16506, .T. ) ;
#17697 = ORIENTED_EDGE ( 'NONE', *, *, #17742, .T. ) ;
#17698 = CARTESIAN_POINT ( 'NONE',  ( -42.50000000000000000, 10.00000000000000000, 44.99999999999999289 ) ) ;
#17699 = LINE ( 'NONE', #20930, #13259 ) ;
#17700 = AXIS2_PLACEMENT_3D ( 'NONE', #2376, #12670, #9241 ) ;
#17701 = DIRECTION ( 'NONE',  ( -1.000000000000000000, 0.000000000000000000, 0.000000000000000000 ) ) ;
#17702 = ADVANCED_FACE ( 'NONE', ( #7882 ), #19913, .T. ) ;
#17703 = CIRCLE ( 'NONE', #1971, 36.76383501243555685 ) ;
#17704 = DIRECTION ( 'NONE',  ( 0.000000000000000000, 0.000000000000000000, -1.000000000000000000 ) ) ;
#17705 = FACE_OUTER_BOUND ( 'NONE', #14502, .T. ) ;
#17706 = CARTESIAN_POINT ( 'NONE',  ( 4.585174426381384727, 39.86909732867421496, 51.95486263624831480 ) ) ;
#17707 = AXIS2_PLACEMENT_3D ( 'NONE', #14878, #6537, #8140 ) ;
#17708 = VERTEX_POINT ( 'NONE', #7422 ) ;
#17709 = FACE_OUTER_BOUND ( 'NONE', #2810, .T. ) ;
#17710 = CARTESIAN_POINT ( 'NONE',  ( 13.00000000000024336, -2.516660498395250745, 100.0000000000000000 ) ) ;
#17711 = DIRECTION ( 'NONE',  ( -0.000000000000000000, 1.000000000000000000, -0.000000000000000000 ) ) ;
#17712 = ADVANCED_FACE ( 'NONE', ( #3887 ), #14394, .F. ) ;
#17713 = CARTESIAN_POINT ( 'NONE',  ( 13.85640646055118808, -1.500000000000015099, 7.999999999999710454 ) ) ;
#17714 = ADVANCED_FACE ( 'NONE', ( #546 ), #11195, .F. ) ;
#17715 = AXIS2_PLACEMENT_3D ( 'NONE', #21103, #8835, #13749 ) ;
#17716 = DIRECTION ( 'NONE',  ( 0.000000000000000000, 0.000000000000000000, -1.000000000000000000 ) ) ;
#17717 = AXIS2_PLACEMENT_3D ( 'NONE', #4101, #11071, #9370 ) ;
#17718 = DIRECTION ( 'NONE',  ( 1.296372316667914327E-16, 1.000000000000000000, -0.000000000000000000 ) ) ;
#17719 = DIRECTION ( 'NONE',  ( 1.000000000000000000, 0.000000000000000000, 0.000000000000000000 ) ) ;
#17720 = EDGE_CURVE ( 'NONE', #16652, #16333, #6556, .T. ) ;
#17721 = MANIFOLD_SOLID_BREP ( 'Chamfer3', #7857 ) ;
#17722 = ORIENTED_EDGE ( 'NONE', *, *, #1206, .T. ) ;
#17723 = ADVANCED_FACE ( 'NONE', ( #3305 ), #6923, .T. ) ;
#17724 = ORIENTED_EDGE ( 'NONE', *, *, #12562, .F. ) ;
#17725 = EDGE_CURVE ( 'NONE', #11729, #21259, #19104, .T. ) ;
#17726 = ORIENTED_EDGE ( 'NONE', *, *, #7371, .T. ) ;
#17727 = CARTESIAN_POINT ( 'NONE',  ( 8.523345606290934739, -2.856915207368400988, -52.89411661619065086 ) ) ;
#17728 = ADVANCED_FACE ( 'NONE', ( #19339 ), #7173, .F. ) ;
#17729 = CYLINDRICAL_SURFACE ( 'NONE', #14156, 36.76383501243555685 ) ;
#17730 = CONICAL_SURFACE ( 'NONE', #6766, 2.524999999999999467, 0.7853981633974482790 ) ;
#17731 = FACE_OUTER_BOUND ( 'NONE', #18591, .T. ) ;
#17732 = DIRECTION ( 'NONE',  ( -6.505213034913038160E-19, -3.903127820947822896E-18, -1.000000000000000000 ) ) ;
#17733 = DIRECTION ( 'NONE',  ( 0.000000000000000000, 0.000000000000000000, 1.000000000000000000 ) ) ;
#17734 = CARTESIAN_POINT ( 'NONE',  ( -19.42347305479418296, 31.41593231561366650, -57.95407386126544225 ) ) ;
#17735 = DIRECTION ( 'NONE',  ( 0.000000000000000000, -1.000000000000000000, 0.000000000000000000 ) ) ;
#17736 = EDGE_LOOP ( 'NONE', ( #6913, #8490, #1145, #27 ) ) ;
#17737 = FACE_OUTER_BOUND ( 'NONE', #8626, .T. ) ;
#17738 = LINE ( 'NONE', #9034, #22503 ) ;
#17739 = CARTESIAN_POINT ( 'NONE',  ( 3.330669073875469621E-13, -1.110223024625156540E-13, -2.999999999999971578 ) ) ;
#17740 = VECTOR ( 'NONE', #7766, 1000.000000000000000 ) ;
#17741 = FACE_BOUND ( 'NONE', #6356, .T. ) ;
#17742 = EDGE_CURVE ( 'NONE', #10689, #2580, #16057, .T. ) ;
#17743 = VERTEX_POINT ( 'NONE', #178 ) ;
#17744 = EDGE_CURVE ( 'NONE', #8376, #12666, #10929, .T. ) ;
#17745 = AXIS2_PLACEMENT_3D ( 'NONE', #18513, #6483, #6370 ) ;
#17746 = CARTESIAN_POINT ( 'NONE',  ( -42.50000000000000000, 10.00000000000000000, 49.99999999999999289 ) ) ;
#17747 = DIRECTION ( 'NONE',  ( 0.000000000000000000, 0.000000000000000000, -1.000000000000000000 ) ) ;
#17748 = CARTESIAN_POINT ( 'NONE',  ( 13.56354382738798137, 2.142135623730915928, -56.03997097393683902 ) ) ;
#17749 = CIRCLE ( 'NONE', #16288, 2.999999999999999112 ) ;
#17750 = EDGE_CURVE ( 'NONE', #15308, #9422, #702, .T. ) ;
#17751 = VERTEX_POINT ( 'NONE', #8555 ) ;
#17752 = MANIFOLD_SOLID_BREP ( 'Boss-Extrude1', #3484 ) ;
#17753 = AXIS2_PLACEMENT_3D ( 'NONE', #3806, #10436, #361 ) ;
#17754 = ORIENTED_EDGE ( 'NONE', *, *, #13510, .F. ) ;
#17755 = CARTESIAN_POINT ( 'NONE',  ( 0.1964561668385597371, 39.99977788401218959, -48.88630801547629545 ) ) ;
#17756 = AXIS2_PLACEMENT_3D ( 'NONE', #9030, #5827, #18070 ) ;
#17757 = DIRECTION ( 'NONE',  ( -0.000000000000000000, -1.000000000000000000, -0.000000000000000000 ) ) ;
#17758 = CARTESIAN_POINT ( 'NONE',  ( -28.95348479018550236, 14.76298474240492276, -6.999999999999950262 ) ) ;
#17759 = VERTEX_POINT ( 'NONE', #19450 ) ;
#17760 = CARTESIAN_POINT ( 'NONE',  ( -35.00000000000000000, 17.00000000000000000, -38.99999999999999289 ) ) ;
#17761 = CARTESIAN_POINT ( 'NONE',  ( -7.392691288592804000, 39.99999999999999289, 52.71482085253978056 ) ) ;
#17762 = VERTEX_POINT ( 'NONE', #1911 ) ;
#17763 = AXIS2_PLACEMENT_3D ( 'NONE', #5932, #10853, #4341 ) ;
#17764 = DIRECTION ( 'NONE',  ( -6.505213034913038160E-19, -3.903127820947822896E-18, -1.000000000000000000 ) ) ;
#17765 = CARTESIAN_POINT ( 'NONE',  ( 22.43696576003031851, 20.17999529786815671, -58.67002796852975166 ) ) ;
#17766 = CIRCLE ( 'NONE', #7532, 6.499999999999999112 ) ;
#17767 = DIRECTION ( 'NONE',  ( 6.505213034913038160E-19, 3.903127820947822896E-18, 1.000000000000000000 ) ) ;
#17768 = EDGE_LOOP ( 'NONE', ( #9776, #132, #21412, #13435 ) ) ;
#17769 = DIRECTION ( 'NONE',  ( -6.505213034913038160E-19, -3.903127820947822896E-18, -1.000000000000000000 ) ) ;
#17770 = CARTESIAN_POINT ( 'NONE',  ( -11.86180952233172725, 39.00000000000000000, -55.35904751184885697 ) ) ;
#17771 = CARTESIAN_POINT ( 'NONE',  ( -1.038203980847386187, 39.99359456186276418, -49.52478356376864355 ) ) ;
#17772 = EDGE_CURVE ( 'NONE', #4267, #20199, #10701, .T. ) ;
#17773 = ORIENTED_EDGE ( 'NONE', *, *, #9393, .F. ) ;
#17774 = DIRECTION ( 'NONE',  ( 6.505213034913038160E-19, 3.903127820947822896E-18, 1.000000000000000000 ) ) ;
#17775 = DIRECTION ( 'NONE',  ( -6.505213034913038160E-19, -3.903127820947822896E-18, -1.000000000000000000 ) ) ;
#17776 = VECTOR ( 'NONE', #14686, 1000.000000000000000 ) ;
#17777 = CIRCLE ( 'NONE', #9362, 19.11328065563152379 ) ;
#17778 = CIRCLE ( 'NONE', #20716, 0.9999999999999974465 ) ;
#17779 = ORIENTED_EDGE ( 'NONE', *, *, #19931, .T. ) ;
#17780 = AXIS2_PLACEMENT_3D ( 'NONE', #9505, #14642, #22104 ) ;
#17781 = VERTEX_POINT ( 'NONE', #7744 ) ;
#17782 = ORIENTED_EDGE ( 'NONE', *, *, #1499, .F. ) ;
#17783 = EDGE_CURVE ( 'NONE', #14167, #131, #3283, .T. ) ;
#17784 = ORIENTED_EDGE ( 'NONE', *, *, #19552, .F. ) ;
#17785 = CARTESIAN_POINT ( 'NONE',  ( 2.775557561562891351E-14, -2.775557561562891351E-14, 2.999999999999995559 ) ) ;
#17786 = FACE_OUTER_BOUND ( 'NONE', #7221, .T. ) ;
#17787 = APPLICATION_CONTEXT ( 'automotive_design' ) ;
#17788 = CARTESIAN_POINT ( 'NONE',  ( -29.74882400976398955, -20.54749497201925479, 2.932969818539056028 ) ) ;
#17789 = CARTESIAN_POINT ( 'NONE',  ( 25.00000000000000000, 20.00000000000000000, 6.487780019669002523E-15 ) ) ;
#17790 = ORIENTED_EDGE ( 'NONE', *, *, #4077, .T. ) ;
#17791 = CARTESIAN_POINT ( 'NONE',  ( 3.330669073875469621E-13, -1.110223024625156540E-13, -2.999999999999971578 ) ) ;
#17792 = DIRECTION ( 'NONE',  ( -0.000000000000000000, -1.000000000000000000, -0.000000000000000000 ) ) ;
#17793 = ORIENTED_EDGE ( 'NONE', *, *, #17824, .T. ) ;
#17794 = AXIS2_PLACEMENT_3D ( 'NONE', #14078, #22610, #2071 ) ;
#17795 = CIRCLE ( 'NONE', #9010, 34.90673715956759082 ) ;
#17796 = CARTESIAN_POINT ( 'NONE',  ( -1.799800578957587716, 0.06826247860514957078, 51.82705267766674950 ) ) ;
#17797 = VECTOR ( 'NONE', #19053, 1000.000000000000000 ) ;
#17798 = CARTESIAN_POINT ( 'NONE',  ( -12.23364788621111643, 38.77571842908470501, -55.51446324382121134 ) ) ;
#17799 = AXIS2_PLACEMENT_3D ( 'NONE', #6538, #11688, #2989 ) ;
#17800 = EDGE_CURVE ( 'NONE', #13632, #18629, #16337, .T. ) ;
#17801 = LINE ( 'NONE', #2101, #10854 ) ;
#17802 = EDGE_LOOP ( 'NONE', ( #15381, #14596, #7225, #21207 ) ) ;
#17803 = CARTESIAN_POINT ( 'NONE',  ( 1.061447036142194600, 34.97146889883303800, 38.77662560222201904 ) ) ;
#17804 = VERTEX_POINT ( 'NONE', #15989 ) ;
#17805 = CARTESIAN_POINT ( 'NONE',  ( -19.99999999999999289, -2.799736964075212609E-14, 2.999999999999995559 ) ) ;
#17806 = MANIFOLD_SOLID_BREP ( 'Revolve1', #1646 ) ;
#17807 = CARTESIAN_POINT ( 'NONE',  ( 2.220446049250313081E-13, -2.498001805406602216E-13, -6.859353255829918616 ) ) ;
#17808 = CARTESIAN_POINT ( 'NONE',  ( 6.263166516349132351, 0.9587459495540682219, 54.84564255054416293 ) ) ;
#17809 = AXIS2_PLACEMENT_3D ( 'NONE', #18054, #9360, #16342 ) ;
#17810 = CARTESIAN_POINT ( 'NONE',  ( 19.59396665412829464, 15.89499847339836691, 60.52448832957817615 ) ) ;
#17811 = CARTESIAN_POINT ( 'NONE',  ( -16.06969024216325792, -19.15111107797470780, -4.999999999999969802 ) ) ;
#17812 = CIRCLE ( 'NONE', #2824, 3.000000000000002665 ) ;
#17813 = EDGE_LOOP ( 'NONE', ( #20524, #14358, #4912, #9105 ) ) ;
#17814 = EDGE_LOOP ( 'NONE', ( #7768, #9430, #6713, #10934 ) ) ;
#17815 = ORIENTED_EDGE ( 'NONE', *, *, #4299, .F. ) ;
#17816 = EDGE_CURVE ( 'NONE', #18632, #17095, #1804, .T. ) ;
#17817 = ORIENTED_EDGE ( 'NONE', *, *, #15453, .F. ) ;
#17818 = CARTESIAN_POINT ( 'NONE',  ( 35.00000000000000000, -5.000000000000000000, 57.00000000000002842 ) ) ;
#17819 = AXIS2_PLACEMENT_3D ( 'NONE', #18193, #20035, #2507 ) ;
#17820 = FACE_OUTER_BOUND ( 'NONE', #9659, .T. ) ;
#17821 = DIRECTION ( 'NONE',  ( -0.000000000000000000, 1.000000000000000000, -0.000000000000000000 ) ) ;
#17822 = FACE_OUTER_BOUND ( 'NONE', #21225, .T. ) ;
#17823 = CYLINDRICAL_SURFACE ( 'NONE', #17596, 19.11328065563151668 ) ;
#17824 = EDGE_CURVE ( 'NONE', #8988, #15447, #12045, .T. ) ;
#17825 = ORIENTED_EDGE ( 'NONE', *, *, #15510, .T. ) ;
#17826 = CARTESIAN_POINT ( 'NONE',  ( 12.09218358684860917, 1.291952833854519422, -55.42846997241216656 ) ) ;
#17827 = AXIS2_PLACEMENT_3D ( 'NONE', #5737, #3796, #10757 ) ;
#17828 = CARTESIAN_POINT ( 'NONE',  ( 42.50000000000000000, 7.000000000000000000, 44.99999999999999289 ) ) ;
#17829 = CIRCLE ( 'NONE', #22609, 2.099999999999997868 ) ;
#17830 = FACE_OUTER_BOUND ( 'NONE', #17428, .T. ) ;
#17831 = CARTESIAN_POINT ( 'NONE',  ( -35.00000000000058265, 26.00000000000000355, -52.90000000000076597 ) ) ;
#17832 = DIRECTION ( 'NONE',  ( 8.659560562354903276E-17, -0.7071067811865500152, 0.7071067811865451302 ) ) ;
#17833 = FACE_OUTER_BOUND ( 'NONE', #19377, .T. ) ;
#17834 = EDGE_CURVE ( 'NONE', #10145, #18993, #21948, .T. ) ;
#17835 = TOROIDAL_SURFACE ( 'NONE', #21873, 34.90673715956759082, 8.750000000000000000 ) ;
#17836 = AXIS2_PLACEMENT_3D ( 'NONE', #4733, #8154, #15008 ) ;
#17837 = DIRECTION ( 'NONE',  ( -0.000000000000000000, -0.000000000000000000, 1.000000000000000000 ) ) ;
#17838 = EDGE_LOOP ( 'NONE', ( #4424, #7378, #1423, #13538, #536, #3264, #13533, #7450, #418 ) ) ;
#17839 = VERTEX_POINT ( 'NONE', #18286 ) ;
#17840 = AXIS2_PLACEMENT_3D ( 'NONE', #12710, #16040, #350 ) ;
#17841 = EDGE_CURVE ( 'NONE', #12474, #14756, #17525, .T. ) ;
#17842 = CIRCLE ( 'NONE', #13060, 57.07106781186551103 ) ;
#17843 = ORIENTED_EDGE ( 'NONE', *, *, #21280, .F. ) ;
#17844 = CARTESIAN_POINT ( 'NONE',  ( -1.564319729173966111, -1.162775034690410214, -47.08282483555584008 ) ) ;
#17845 = CARTESIAN_POINT ( 'NONE',  ( 15.12081897056669000, -33.51030287062373247, -2.800654218530457484 ) ) ;
#17846 = DIRECTION ( 'NONE',  ( 0.000000000000000000, -0.000000000000000000, 1.000000000000000000 ) ) ;
#17847 = AXIS2_PLACEMENT_3D ( 'NONE', #20838, #19110, #1812 ) ;
#17848 = ADVANCED_FACE ( 'NONE', ( #14376 ), #9007, .F. ) ;
#17849 = DIRECTION ( 'NONE',  ( 0.000000000000000000, -1.000000000000000000, 0.000000000000000000 ) ) ;
#17850 = CARTESIAN_POINT ( 'NONE',  ( 0.000000000000000000, 30.00000000000000355, 0.000000000000000000 ) ) ;
#17851 = LINE ( 'NONE', #7314, #3598 ) ;
#17852 = FACE_OUTER_BOUND ( 'NONE', #22404, .T. ) ;
#17853 = CIRCLE ( 'NONE', #13099, 31.50000000000001421 ) ;
#17854 = AXIS2_PLACEMENT_3D ( 'NONE', #3432, #8466, #13851 ) ;
#17855 = ORIENTED_EDGE ( 'NONE', *, *, #5392, .T. ) ;
#17856 = CARTESIAN_POINT ( 'NONE',  ( 90.00000000000000000, 40.00000000000000000, 2.500000000000001332 ) ) ;
#17857 = AXIS2_PLACEMENT_3D ( 'NONE', #15051, #4991, #18970 ) ;
#17858 = CARTESIAN_POINT ( 'NONE',  ( 3.469446951953614189E-15, 38.23275711891355400, 0.000000000000000000 ) ) ;
#17859 = EDGE_CURVE ( 'NONE', #14794, #10996, #412, .T. ) ;
#17860 = CARTESIAN_POINT ( 'NONE',  ( 0.000000000000000000, 10.00000000000000000, 0.000000000000000000 ) ) ;
#17861 = CARTESIAN_POINT ( 'NONE',  ( 10.38193264731109977, 9.167449762519654044, -43.52061562521063109 ) ) ;
#17862 = AXIS2_PLACEMENT_3D ( 'NONE', #2781, #8157, #22142 ) ;
#17863 = VERTEX_POINT ( 'NONE', #7297 ) ;
#17864 = ADVANCED_FACE ( 'NONE', ( #18174 ), #21274, .F. ) ;
#17865 = CARTESIAN_POINT ( 'NONE',  ( -9.708269511265271490, 33.52953626616022831, 2.999999999999999112 ) ) ;
#17866 = CARTESIAN_POINT ( 'NONE',  ( -9.165151389911720514, 40.00000000000000000, 56.36098470834082264 ) ) ;
#17867 = CARTESIAN_POINT ( 'NONE',  ( -35.00000000000000000, 0.000000000000000000, 2.365113165210053967E-14 ) ) ;
#17868 = ADVANCED_FACE ( 'NONE', ( #17830 ), #9473, .T. ) ;
#17869 = EDGE_LOOP ( 'NONE', ( #20111, #15517, #1878, #188 ) ) ;
#17870 = VECTOR ( 'NONE', #7287, 1000.000000000000000 ) ;
#17871 = VECTOR ( 'NONE', #9491, 1000.000000000000000 ) ;
#17872 = AXIS2_PLACEMENT_3D ( 'NONE', #13769, #3263, #8516 ) ;
#17873 = EDGE_CURVE ( 'NONE', #6208, #1794, #16191, .T. ) ;
#17874 = ORIENTED_EDGE ( 'NONE', *, *, #7254, .T. ) ;
#17875 = CARTESIAN_POINT ( 'NONE',  ( -2.999999999999999556, 22.00000000000000355, 8.485281374238567764 ) ) ;
#17876 = DIRECTION ( 'NONE',  ( 1.000000000000000000, 0.000000000000000000, 0.000000000000000000 ) ) ;
#17877 = DIRECTION ( 'NONE',  ( 6.505213034913038160E-19, 3.903127820947822896E-18, 1.000000000000000000 ) ) ;
#17878 = ADVANCED_FACE ( 'NONE', ( #11855 ), #1439, .T. ) ;
#17879 = ORIENTED_EDGE ( 'NONE', *, *, #12200, .T. ) ;
#17880 = CARTESIAN_POINT ( 'NONE',  ( 7.094908322883425100, -35.33352588067118205, 2.999999999999995559 ) ) ;
#17881 = FACE_OUTER_BOUND ( 'NONE', #16553, .T. ) ;
#17882 = ORIENTED_EDGE ( 'NONE', *, *, #20419, .F. ) ;
#17883 = DIRECTION ( 'NONE',  ( -0.000000000000000000, 1.000000000000000000, -0.000000000000000000 ) ) ;
#17884 = CARTESIAN_POINT ( 'NONE',  ( 0.000000000000000000, -45.00000000000000000, 0.000000000000000000 ) ) ;
#17885 = CARTESIAN_POINT ( 'NONE',  ( -34.99999999999999289, -5.000000000000000000, -3.012171160963566127E-14 ) ) ;
#17886 = DIRECTION ( 'NONE',  ( 0.000000000000000000, 1.000000000000000000, 0.000000000000000000 ) ) ;
#17887 = PRESENTATION_LAYER_ASSIGNMENT (  '', '', ( #13126 ) ) ;
#17888 = ORIENTED_EDGE ( 'NONE', *, *, #7381, .T. ) ;
#17889 = FACE_OUTER_BOUND ( 'NONE', #582, .T. ) ;
#17890 = FACE_OUTER_BOUND ( 'NONE', #8800, .T. ) ;
#17891 = CIRCLE ( 'NONE', #683, 1.000000000000000888 ) ;
#17892 = CARTESIAN_POINT ( 'NONE',  ( -6.501355175172208511, 39.72712728739963239, -53.07780961191252089 ) ) ;
#17893 = VERTEX_POINT ( 'NONE', #16905 ) ;
#17894 = DIRECTION ( 'NONE',  ( -1.000000000000000000, 0.000000000000000000, 0.000000000000000000 ) ) ;
#17895 = FACE_OUTER_BOUND ( 'NONE', #11024, .T. ) ;
#17896 = DIRECTION ( 'NONE',  ( 1.000000000000000000, 1.208970125616065955E-17, 0.000000000000000000 ) ) ;
#17897 = PRODUCT_DEFINITION_FORMATION_WITH_SPECIFIED_SOURCE ( 'ANY', '', #12944, .NOT_KNOWN. ) ;
#17898 = EDGE_LOOP ( 'NONE', ( #8877, #9516, #20942, #5179 ) ) ;
#17899 = ORIENTED_EDGE ( 'NONE', *, *, #3987, .F. ) ;
#17900 = AXIS2_PLACEMENT_3D ( 'NONE', #5833, #12797, #19812 ) ;
#17901 = EDGE_LOOP ( 'NONE', ( #5108, #7737, #21754, #18952 ) ) ;
#17902 = ADVANCED_FACE ( 'NONE', ( #2599 ), #4371, .F. ) ;
#17903 = VERTEX_POINT ( 'NONE', #11526 ) ;
#17904 = DIRECTION ( 'NONE',  ( 8.659560562351929024E-17, -0.7071067811867928210, 0.7071067811863022134 ) ) ;
#17905 = DIRECTION ( 'NONE',  ( 0.000000000000000000, 0.000000000000000000, 1.000000000000000000 ) ) ;
#17906 = LINE ( 'NONE', #17669, #8459 ) ;
#17907 = DIRECTION ( 'NONE',  ( -1.000000000000000000, -1.208970125616063644E-17, 0.000000000000000000 ) ) ;
#17908 = EDGE_LOOP ( 'NONE', ( #4269, #14932, #17471, #9437 ) ) ;
#17909 = DIRECTION ( 'NONE',  ( -1.000000000000000000, -0.000000000000000000, -0.000000000000000000 ) ) ;
#17910 = CARTESIAN_POINT ( 'NONE',  ( 36.06598984771572702, 10.00000000000000000, -48.42385786802028491 ) ) ;
#17911 = ORIENTED_EDGE ( 'NONE', *, *, #18661, .T. ) ;
#17912 = CARTESIAN_POINT ( 'NONE',  ( 25.00000000000000000, 20.00000000000000000, -24.99999999999999289 ) ) ;
#17913 = CYLINDRICAL_SURFACE ( 'NONE', #14107, 36.76383501243555685 ) ;
#17914 = CYLINDRICAL_SURFACE ( 'NONE', #7952, 2.500000000000002220 ) ;
#17915 = ORIENTED_EDGE ( 'NONE', *, *, #14528, .T. ) ;
#17916 = DIRECTION ( 'NONE',  ( -6.505213034913038160E-19, -3.903127820947822896E-18, -1.000000000000000000 ) ) ;
#17917 = EDGE_CURVE ( 'NONE', #8015, #13677, #1321, .T. ) ;
#17918 = ORIENTED_EDGE ( 'NONE', *, *, #19649, .T. ) ;
#17919 = DIRECTION ( 'NONE',  ( 0.000000000000000000, 0.000000000000000000, 1.000000000000000000 ) ) ;
#17920 = DIRECTION ( 'NONE',  ( 0.000000000000000000, 0.000000000000000000, -1.000000000000000000 ) ) ;
#17921 = ORIENTED_EDGE ( 'NONE', *, *, #9526, .T. ) ;
#17922 = AXIS2_PLACEMENT_3D ( 'NONE', #20152, #2627, #2735 ) ;
#17923 = CARTESIAN_POINT ( 'NONE',  ( 18.14075711706860616, 28.59859666635273001, 57.62969612438692479 ) ) ;
#17924 = FACE_OUTER_BOUND ( 'NONE', #9676, .T. ) ;
#17925 = DIRECTION ( 'NONE',  ( -0.5002637533272176196, 0.000000000000000000, 0.8658730721687590837 ) ) ;
#17926 = ORIENTED_EDGE ( 'NONE', *, *, #11607, .F. ) ;
#17927 = ADVANCED_FACE ( 'NONE', ( #6367 ), #1453, .T. ) ;
#17928 = CIRCLE ( 'NONE', #15363, 5.000000000000000000 ) ;
#17929 = ORIENTED_EDGE ( 'NONE', *, *, #19340, .F. ) ;
#17930 = VERTEX_POINT ( 'NONE', #14827 ) ;
#17931 = ORIENTED_EDGE ( 'NONE', *, *, #3059, .T. ) ;
#17932 = DIRECTION ( 'NONE',  ( 6.505213034913038160E-19, 3.903127820947822896E-18, 1.000000000000000000 ) ) ;
#17933 = DIRECTION ( 'NONE',  ( -1.000000000000000000, 0.000000000000000000, -0.000000000000000000 ) ) ;
#17934 = CARTESIAN_POINT ( 'NONE',  ( -15.00354810072192713, 32.89319786336240981, -2.933296326616371186 ) ) ;
#17935 = VECTOR ( 'NONE', #13237, 1000.000000000000114 ) ;
#17936 = ORIENTED_EDGE ( 'NONE', *, *, #2427, .F. ) ;
#17937 = DIRECTION ( 'NONE',  ( 6.505213034913038160E-19, 3.903127820947822896E-18, 1.000000000000000000 ) ) ;
#17938 = CARTESIAN_POINT ( 'NONE',  ( -20.36304159388342683, -24.03323817228481118, -2.999999999999999112 ) ) ;
#17939 = ORIENTED_EDGE ( 'NONE', *, *, #9134, .F. ) ;
#17940 = DIRECTION ( 'NONE',  ( 1.000000000000000000, 0.000000000000000000, 0.000000000000000000 ) ) ;
#17941 = CARTESIAN_POINT ( 'NONE',  ( -18.65063509461084479, 12.49999999999990052, -2.999999999999988898 ) ) ;
#17942 = CARTESIAN_POINT ( 'NONE',  ( 6.742883674876798850, 34.24928931925757780, -2.999999999999971578 ) ) ;
#17943 = CARTESIAN_POINT ( 'NONE',  ( 2.999999999999997780, 30.00000000000000000, 6.485281374238567764 ) ) ;
#17944 = VECTOR ( 'NONE', #18673, 1000.000000000000000 ) ;
#17945 = FACE_OUTER_BOUND ( 'NONE', #20155, .T. ) ;
#17946 = EDGE_CURVE ( 'NONE', #7291, #15608, #11331, .T. ) ;
#17947 = PRODUCT_DEFINITION ( 'UNKNOWN', '', #17530, #10949 ) ;
#17948 = CARTESIAN_POINT ( 'NONE',  ( -5.204793789172661889, 39.83796802612397414, 52.32473130827783336 ) ) ;
#17949 = CARTESIAN_POINT ( 'NONE',  ( 2.775557561562891351E-14, -2.775557561562891351E-14, 2.999999999999999112 ) ) ;
#17950 = ORIENTED_EDGE ( 'NONE', *, *, #12040, .F. ) ;
#17951 = EDGE_CURVE ( 'NONE', #16045, #104, #10412, .T. ) ;
#17952 = VERTEX_POINT ( 'NONE', #18390 ) ;
#17953 = B_SPLINE_CURVE_WITH_KNOTS ( 'NONE', 3,
 ( #8249, #3337, #15221, #1720 ),
 .UNSPECIFIED., .F., .F.,
 ( 4, 4 ),
 ( 0.001875451646902988193, 0.003761979286331204771 ),
 .UNSPECIFIED. ) ;
#17954 = ORIENTED_EDGE ( 'NONE', *, *, #5379, .T. ) ;
#17955 = CARTESIAN_POINT ( 'NONE',  ( 35.00000000000000000, 40.00000000000000000, 4.258610482196280173E-15 ) ) ;
#17956 = AXIS2_PLACEMENT_3D ( 'NONE', #4083, #7510, #4193 ) ;
#17957 = CARTESIAN_POINT ( 'NONE',  ( -7.882609639814679786E-15, -9.552912840896525389E-26, -50.50395615645409464 ) ) ;
#17958 = CARTESIAN_POINT ( 'NONE',  ( 35.00000000000000000, -5.000000000000000000, 57.49999999999698730 ) ) ;
#17959 = DIRECTION ( 'NONE',  ( 0.000000000000000000, 1.000000000000000000, 0.000000000000000000 ) ) ;
#17960 = EDGE_CURVE ( 'NONE', #7926, #1702, #9914, .T. ) ;
#17961 = DIRECTION ( 'NONE',  ( -1.000000000000000000, 1.052817288873012122E-14, 0.000000000000000000 ) ) ;
#17962 = SPHERICAL_SURFACE ( 'NONE', #20444, 43.25806096964027603 ) ;
#17963 = CARTESIAN_POINT ( 'NONE',  ( -15.62751878812966133, 32.48885827236730961, -59.38785559521993207 ) ) ;
#17964 = DIRECTION ( 'NONE',  ( -6.505213034913038160E-19, -3.903127820947822896E-18, -1.000000000000000000 ) ) ;
#17965 = VERTEX_POINT ( 'NONE', #14119 ) ;
#17966 = CARTESIAN_POINT ( 'NONE',  ( 17.32050807568884210, 1.500000000000015099, -9.999999999999880984 ) ) ;
#17967 = CYLINDRICAL_SURFACE ( 'NONE', #21202, 2.499999999999998668 ) ;
#17968 = FACE_OUTER_BOUND ( 'NONE', #12750, .T. ) ;
#17969 = ADVANCED_FACE ( 'NONE', ( #4993 ), #12193, .F. ) ;
#17970 = CARTESIAN_POINT ( 'NONE',  ( 29.14949368109903816, -11.93972437435564160, -2.999999999999971578 ) ) ;
#17971 = ORIENTED_EDGE ( 'NONE', *, *, #20146, .T. ) ;
#17972 = FACE_OUTER_BOUND ( 'NONE', #22066, .T. ) ;
#17973 = ORIENTED_EDGE ( 'NONE', *, *, #12763, .T. ) ;
#17974 = CARTESIAN_POINT ( 'NONE',  ( 24.62019382530525391, -4.341204441673157888, -5.000000000000004441 ) ) ;
#17975 = CARTESIAN_POINT ( 'NONE',  ( 92.09999999999999432, 28.00000000000000000, -9.108981535246192915E-16 ) ) ;
#17976 = DIRECTION ( 'NONE',  ( -0.000000000000000000, -1.000000000000000000, -0.000000000000000000 ) ) ;
#17977 = ORIENTED_EDGE ( 'NONE', *, *, #11725, .T. ) ;
#17978 = DIRECTION ( 'NONE',  ( 6.505213034913038160E-19, 3.903127820947822896E-18, 1.000000000000000000 ) ) ;
#17979 = AXIS2_PLACEMENT_3D ( 'NONE', #20976, #11701, #18695 ) ;
#17980 = EDGE_LOOP ( 'NONE', ( #3964, #13572, #2415, #17666 ) ) ;
#17981 = FACE_OUTER_BOUND ( 'NONE', #771, .T. ) ;
#17982 = CARTESIAN_POINT ( 'NONE',  ( 35.00000000000001421, -5.000000000000000000, 1.540743955509788682E-30 ) ) ;
#17983 = EDGE_CURVE ( 'NONE', #6403, #10477, #13859, .T. ) ;
#17984 = DIRECTION ( 'NONE',  ( 1.000000000000000000, 0.000000000000000000, 0.000000000000000000 ) ) ;
#17985 = ORIENTED_EDGE ( 'NONE', *, *, #13596, .F. ) ;
#17986 = DIRECTION ( 'NONE',  ( 0.000000000000000000, 0.7071067811865451302, -0.7071067811865500152 ) ) ;
#17987 = CARTESIAN_POINT ( 'NONE',  ( -7.434571854303535510, 39.99999999999999289, 52.73242012342949181 ) ) ;
#17988 = VERTEX_POINT ( 'NONE', #17461 ) ;
#17989 = DIRECTION ( 'NONE',  ( -0.000000000000000000, -1.000000000000000000, -0.000000000000000000 ) ) ;
#17990 = CYLINDRICAL_SURFACE ( 'NONE', #11973, 2.099999999999990763 ) ;
#17991 = DIRECTION ( 'NONE',  ( -0.000000000000000000, -0.000000000000000000, 1.000000000000000000 ) ) ;
#17992 = DIRECTION ( 'NONE',  ( -0.000000000000000000, -0.000000000000000000, -1.000000000000000000 ) ) ;
#17993 = ORIENTED_EDGE ( 'NONE', *, *, #20926, .T. ) ;
#17994 = CARTESIAN_POINT ( 'NONE',  ( -35.00000000000000000, 0.000000000000000000, 9.000000000000015987 ) ) ;
#17995 = PLANE ( 'NONE',  #1413 ) ;
#17996 = EDGE_CURVE ( 'NONE', #22225, #2199, #17537, .T. ) ;
#17997 = EDGE_CURVE ( 'NONE', #950, #3930, #19081, .T. ) ;
#17998 = CARTESIAN_POINT ( 'NONE',  ( -6.069328110416789990, 39.76463894057638271, -52.83839008176153840 ) ) ;
#17999 = ORIENTED_EDGE ( 'NONE', *, *, #10697, .F. ) ;
#18000 = DIRECTION ( 'NONE',  ( 0.000000000000000000, 0.000000000000000000, -1.000000000000000000 ) ) ;
#18001 = AXIS2_PLACEMENT_3D ( 'NONE', #12825, #21436, #5509 ) ;
#18002 = CARTESIAN_POINT ( 'NONE',  ( -28.50000000000001421, 19.99999999999982947, 100.0000000000000000 ) ) ;
#18003 = EDGE_CURVE ( 'NONE', #15378, #8847, #13998, .T. ) ;
#18004 = ORIENTED_EDGE ( 'NONE', *, *, #20999, .T. ) ;
#18005 = ORIENTED_EDGE ( 'NONE', *, *, #17326, .T. ) ;
#18006 = ORIENTED_EDGE ( 'NONE', *, *, #7110, .F. ) ;
#18007 = VERTEX_POINT ( 'NONE', #12309 ) ;
#18008 = DIRECTION ( 'NONE',  ( -1.000000000000000000, 0.000000000000000000, 0.000000000000000000 ) ) ;
#18009 = LINE ( 'NONE', #5760, #17599 ) ;
#18010 = DIRECTION ( 'NONE',  ( 1.000000000000000000, -1.275531967630005245E-16, 0.000000000000000000 ) ) ;
#18011 = ORIENTED_EDGE ( 'NONE', *, *, #15353, .F. ) ;
#18012 = CARTESIAN_POINT ( 'NONE',  ( -35.00000000000000000, 0.000000000000000000, 39.00000000000002132 ) ) ;
#18013 = CYLINDRICAL_SURFACE ( 'NONE', #14522, 3.000000000000002665 ) ;
#18014 = ORIENTED_EDGE ( 'NONE', *, *, #21853, .F. ) ;
#18015 = DIRECTION ( 'NONE',  ( -1.296372316667914327E-16, -1.000000000000000000, 0.000000000000000000 ) ) ;
#18016 = CARTESIAN_POINT ( 'NONE',  ( -32.27599279215743877, -14.85437171138610957, 3.000000000000055067 ) ) ;
#18017 = EDGE_CURVE ( 'NONE', #17095, #18632, #7306, .T. ) ;
#18018 = DIRECTION ( 'NONE',  ( -0.000000000000000000, -0.000000000000000000, 1.000000000000000000 ) ) ;
#18019 = EDGE_LOOP ( 'NONE', ( #1796, #7214, #932, #19457 ) ) ;
#18020 = DIRECTION ( 'NONE',  ( -6.505213034913038160E-19, -3.903127820947822896E-18, -1.000000000000000000 ) ) ;
#18021 = ORIENTED_EDGE ( 'NONE', *, *, #20591, .F. ) ;
#18022 = DIRECTION ( 'NONE',  ( 1.296372316667914327E-16, 1.000000000000000000, -0.000000000000000000 ) ) ;
#18023 = DIRECTION ( 'NONE',  ( -6.505213034913038160E-19, -3.903127820947822896E-18, -1.000000000000000000 ) ) ;
#18024 = CARTESIAN_POINT ( 'NONE',  ( 2.499203666028194437, 0.1468068017377833490, 52.32025702727163008 ) ) ;
#18025 = VERTEX_POINT ( 'NONE', #19427 ) ;
#18026 = DIRECTION ( 'NONE',  ( -1.000000000000000000, 0.000000000000000000, 0.000000000000000000 ) ) ;
#18027 = CARTESIAN_POINT ( 'NONE',  ( 9.998533603140316472, 40.00000000000000000, 54.54288842742651156 ) ) ;
#18028 = CYLINDRICAL_SURFACE ( 'NONE', #102, 19.11328065563151668 ) ;
#18029 = EDGE_CURVE ( 'NONE', #21858, #599, #13144, .T. ) ;
#18030 = ADVANCED_FACE ( 'NONE', ( #1039 ), #12858, .F. ) ;
#18031 = LINE ( 'NONE', #14592, #1631 ) ;
#18032 = AXIS2_PLACEMENT_3D ( 'NONE', #22048, #13536, #13087 ) ;
#18033 = VERTEX_POINT ( 'NONE', #14232 ) ;
#18034 = ORIENTED_EDGE ( 'NONE', *, *, #17010, .F. ) ;
#18035 = EDGE_CURVE ( 'NONE', #9227, #19871, #12772, .T. ) ;
#18036 = ORIENTED_EDGE ( 'NONE', *, *, #4663, .F. ) ;
#18037 = EDGE_LOOP ( 'NONE', ( #20022, #21974, #11877, #8587 ) ) ;
#18038 = DIRECTION ( 'NONE',  ( -1.000000000000000000, 0.000000000000000000, 0.000000000000000000 ) ) ;
#18039 = LINE ( 'NONE', #4191, #471 ) ;
#18040 = DIRECTION ( 'NONE',  ( -1.000000000000000000, 0.000000000000000000, 0.000000000000000000 ) ) ;
#18041 = ORIENTED_EDGE ( 'NONE', *, *, #9991, .F. ) ;
#18042 = CARTESIAN_POINT ( 'NONE',  ( -11.86180952233172015, 38.99999999999999289, -55.35904751184885697 ) ) ;
#18043 = CARTESIAN_POINT ( 'NONE',  ( -5.816608766684270293, -4.770324936805438121, 49.23968220743370949 ) ) ;
#18044 = CIRCLE ( 'NONE', #20978, 4.000000000000145661 ) ;
#18045 = ORIENTED_EDGE ( 'NONE', *, *, #18426, .T. ) ;
#18046 = CARTESIAN_POINT ( 'NONE',  ( -11.68090480754633731, 3.765577839755393619, -57.90797000640141334 ) ) ;
#18047 = AXIS2_PLACEMENT_3D ( 'NONE', #16079, #7606, #14586 ) ;
#18048 = CARTESIAN_POINT ( 'NONE',  ( -42.50000000000000711, -12.00000000000000000, -54.00000000000000000 ) ) ;
#18049 = CARTESIAN_POINT ( 'NONE',  ( -42.50000000000000711, -9.600000000000001421, 47.50000000000000711 ) ) ;
#18050 = DIRECTION ( 'NONE',  ( 0.000000000000000000, 0.000000000000000000, -1.000000000000000000 ) ) ;
#18051 = VECTOR ( 'NONE', #10895, 1000.000000000000000 ) ;
#18052 = CARTESIAN_POINT ( 'NONE',  ( 42.50000000000000711, -9.600000000000001421, 50.00000000000000711 ) ) ;
#18053 = DIRECTION ( 'NONE',  ( -6.505213034913038160E-19, -3.903127820947822896E-18, -1.000000000000000000 ) ) ;
#18054 = CARTESIAN_POINT ( 'NONE',  ( 25.00000000000000000, 20.00000000000000000, 6.487780019669002523E-15 ) ) ;
#18055 = ORIENTED_EDGE ( 'NONE', *, *, #6484, .F. ) ;
#18056 = AXIS2_PLACEMENT_3D ( 'NONE', #16327, #10696, #12426 ) ;
#18057 = ORIENTED_EDGE ( 'NONE', *, *, #15554, .F. ) ;
#18058 = CONICAL_SURFACE ( 'NONE', #15115, 2.525000000000110489, 0.7853981633971014453 ) ;
#18059 = CONICAL_SURFACE ( 'NONE', #18427, 58.99999999999994316, 0.7853981633974725929 ) ;
#18060 = VERTEX_POINT ( 'NONE', #493 ) ;
#18061 = DIRECTION ( 'NONE',  ( -1.000000000000000000, 0.000000000000000000, 0.000000000000000000 ) ) ;
#18062 = CARTESIAN_POINT ( 'NONE',  ( 35.00000000000000000, 0.000000000000000000, 4.258610482196280173E-15 ) ) ;
#18063 = CARTESIAN_POINT ( 'NONE',  ( 2.951378045150416796, -1.204966337757524375, -50.23352299313520319 ) ) ;
#18064 = EDGE_CURVE ( 'NONE', #19379, #16333, #14992, .T. ) ;
#18065 = AXIS2_PLACEMENT_3D ( 'NONE', #7837, #19993, #17925 ) ;
#18066 = CARTESIAN_POINT ( 'NONE',  ( 3.608224830031758756E-13, -2.775557561562891351E-14, -4.999999999999997335 ) ) ;
#18067 = DIRECTION ( 'NONE',  ( 6.505213034913038160E-19, 3.903127820947822896E-18, 1.000000000000000000 ) ) ;
#18068 = CARTESIAN_POINT ( 'NONE',  ( -3.981144761549149980, 39.90683190540670466, -51.58239934697316897 ) ) ;
#18069 = DIRECTION ( 'NONE',  ( 1.000000000000000000, 0.000000000000000000, 0.000000000000000000 ) ) ;
#18070 = DIRECTION ( 'NONE',  ( 1.224646799147353700E-16, 0.000000000000000000, -1.000000000000000000 ) ) ;
#18071 = EDGE_CURVE ( 'NONE', #14672, #11367, #1819, .T. ) ;
#18072 = CIRCLE ( 'NONE', #13303, 15.00000000000000000 ) ;
#18073 = ORIENTED_EDGE ( 'NONE', *, *, #2880, .F. ) ;
#18074 = CARTESIAN_POINT ( 'NONE',  ( 3.656418565264357490, 37.07861450834798234, 2.999999999999995559 ) ) ;
#18075 = DIRECTION ( 'NONE',  ( 0.000000000000000000, 0.000000000000000000, 1.000000000000000000 ) ) ;
#18076 = FACE_OUTER_BOUND ( 'NONE', #20758, .T. ) ;
#18077 = FACE_OUTER_BOUND ( 'NONE', #4756, .T. ) ;
#18078 = CARTESIAN_POINT ( 'NONE',  ( -34.99999999999980815, 40.00000000000000000, 54.99999999999922551 ) ) ;
#18079 = CIRCLE ( 'NONE', #1249, 2.499999999999995115 ) ;
#18080 = ORIENTED_EDGE ( 'NONE', *, *, #4026, .T. ) ;
#18081 = CARTESIAN_POINT ( 'NONE',  ( -35.00000000000000000, -5.000000000000000000, 1.387778780781445676E-14 ) ) ;
#18082 = VERTEX_POINT ( 'NONE', #19528 ) ;
#18083 = CARTESIAN_POINT ( 'NONE',  ( -26.00000000000001421, 19.99999999999982947, 100.0000000000000000 ) ) ;
#18084 = CARTESIAN_POINT ( 'NONE',  ( 0.000000000000000000, 0.000000000000000000, 0.000000000000000000 ) ) ;
#18085 =( REPRESENTATION_RELATIONSHIP ('NONE','NONE', #8442, #6502 ) REPRESENTATION_RELATIONSHIP_WITH_TRANSFORMATION ( #9049 )SHAPE_REPRESENTATION_RELATIONSHIP( ) );
#18086 = VECTOR ( 'NONE', #4849, 1000.000000000000000 ) ;
#18087 = ORIENTED_EDGE ( 'NONE', *, *, #6028, .T. ) ;
#18088 = VECTOR ( 'NONE', #9720, 1000.000000000000000 ) ;
#18089 = DIRECTION ( 'NONE',  ( 0.000000000000000000, 0.000000000000000000, 1.000000000000000000 ) ) ;
#18090 = MANIFOLD_SOLID_BREP ( 'Cut-Extrude2', #905 ) ;
#18091 = CARTESIAN_POINT ( 'NONE',  ( 7.364743364090521105, 39.99999999999998579, -52.70305476081712470 ) ) ;
#18092 = EDGE_CURVE ( 'NONE', #8965, #16, #2165, .T. ) ;
#18093 = ORIENTED_EDGE ( 'NONE', *, *, #7301, .F. ) ;
#18094 = CARTESIAN_POINT ( 'NONE',  ( 0.7857880201100436723, 12.99916404495491307, 9.000278651541815833 ) ) ;
#18095 = DIRECTION ( 'NONE',  ( 6.505213034913038160E-19, 3.903127820947822896E-18, 1.000000000000000000 ) ) ;
#18096 = CARTESIAN_POINT ( 'NONE',  ( -35.00000000000000000, 39.00000000000000711, 1.387778780781445676E-14 ) ) ;
#18097 = VERTEX_POINT ( 'NONE', #10800 ) ;
#18098 = CARTESIAN_POINT ( 'NONE',  ( 1.387778780781445676E-14, -5.000000000000000000, -1.506085580481783063E-14 ) ) ;
#18099 = CYLINDRICAL_SURFACE ( 'NONE', #15656, 2.999999999999999112 ) ;
#18100 = ORIENTED_EDGE ( 'NONE', *, *, #8571, .F. ) ;
#18101 = CARTESIAN_POINT ( 'NONE',  ( 0.000000000000000000, -45.00000000000000000, 0.000000000000000000 ) ) ;
#18102 = CARTESIAN_POINT ( 'NONE',  ( -8.410506002219646504, 40.00000000000000711, 53.12343481204283080 ) ) ;
#18103 = ADVANCED_FACE ( 'NONE', ( #12138 ), #10622, .F. ) ;
#18104 = DIRECTION ( 'NONE',  ( 0.000000000000000000, 1.000000000000000000, -0.000000000000000000 ) ) ;
#18105 = VERTEX_POINT ( 'NONE', #3440 ) ;
#18106 = DIRECTION ( 'NONE',  ( 1.000000000000000000, 0.000000000000000000, 0.000000000000000000 ) ) ;
#18107 = CIRCLE ( 'NONE', #5663, 34.90673715956759082 ) ;
#18108 = CARTESIAN_POINT ( 'NONE',  ( 2.220446049250313081E-13, -2.498001805406602216E-13, -6.859353255829918616 ) ) ;
#18109 = CARTESIAN_POINT ( 'NONE',  ( -2.213007560440093169, 39.97050982720588763, -50.37695298629697049 ) ) ;
#18110 = VECTOR ( 'NONE', #5826, 1000.000000000000000 ) ;
#18111 = ORIENTED_EDGE ( 'NONE', *, *, #3252, .F. ) ;
#18112 = DIRECTION ( 'NONE',  ( -0.000000000000000000, 1.000000000000000000, -0.000000000000000000 ) ) ;
#18113 = CARTESIAN_POINT ( 'NONE',  ( 13.00000000000024336, -2.516660498395250745, -105.0000000000000142 ) ) ;
#18114 = DIRECTION ( 'NONE',  ( 0.000000000000000000, -1.000000000000000000, 0.000000000000000000 ) ) ;
#18115 = EDGE_CURVE ( 'NONE', #1157, #6106, #10222, .T. ) ;
#18116 = VECTOR ( 'NONE', #1180, 1000.000000000000000 ) ;
#18117 = ORIENTED_EDGE ( 'NONE', *, *, #9393, .T. ) ;
#18118 = CIRCLE ( 'NONE', #21413, 58.99999999999700862 ) ;
#18119 = ORIENTED_EDGE ( 'NONE', *, *, #16444, .T. ) ;
#18120 = VERTEX_POINT ( 'NONE', #17628 ) ;
#18121 = DIRECTION ( 'NONE',  ( 0.9771751164103699150, 0.2123993136968479190, 0.003914512675672810436 ) ) ;
#18122 = ADVANCED_FACE ( 'NONE', ( #1933 ), #18281, .F. ) ;
#18123 = EDGE_CURVE ( 'NONE', #1794, #19351, #15329, .T. ) ;
#18124 = ORIENTED_EDGE ( 'NONE', *, *, #15877, .F. ) ;
#18125 = CARTESIAN_POINT ( 'NONE',  ( 19.99999999999998224, 20.97067337953453858, -60.62177826491070221 ) ) ;
#18126 = AXIS2_PLACEMENT_3D ( 'NONE', #20486, #9932, #22432 ) ;
#18127 = CARTESIAN_POINT ( 'NONE',  ( 3.330669073875469621E-13, -1.110223024625156540E-13, -2.999999999999971578 ) ) ;
#18128 = CARTESIAN_POINT ( 'NONE',  ( 6.215609608695158883, 39.75345721999698867, -52.92319077873423794 ) ) ;
#18129 = DIRECTION ( 'NONE',  ( -0.000000000000000000, -0.000000000000000000, 1.000000000000000000 ) ) ;
#18130 = DIRECTION ( 'NONE',  ( 8.659560562351929024E-17, -0.7071067811867928210, 0.7071067811863022134 ) ) ;
#18131 = ORIENTED_EDGE ( 'NONE', *, *, #19732, .F. ) ;
#18132 = CARTESIAN_POINT ( 'NONE',  ( 21.66577056626875475, -3.820259908672546167, 3.000000000000009770 ) ) ;
#18133 = CYLINDRICAL_SURFACE ( 'NONE', #13802, 10.00000000000000178 ) ;
#18134 = EDGE_LOOP ( 'NONE', ( #11611, #18543, #22078, #21370 ) ) ;
#18135 = CARTESIAN_POINT ( 'NONE',  ( -0.3688098923350720537, -0.009433325537011738246, 50.78496022600280924 ) ) ;
#18136 = DIRECTION ( 'NONE',  ( -1.000000000000000000, -1.208970125616083366E-17, 0.000000000000000000 ) ) ;
#18137 = CARTESIAN_POINT ( 'NONE',  ( 4.918774254215884767, -31.11359284679388182, -2.999999999999999112 ) ) ;
#18138 = EDGE_LOOP ( 'NONE', ( #4208, #2051, #21235, #18934 ) ) ;
#18139 = DIRECTION ( 'NONE',  ( -6.505213034913038160E-19, -3.903127820947822896E-18, -1.000000000000000000 ) ) ;
#18140 = DIRECTION ( 'NONE',  ( -1.000000000000000000, -1.208970125616077665E-17, 0.000000000000000000 ) ) ;
#18141 = ORIENTED_EDGE ( 'NONE', *, *, #3874, .F. ) ;
#18142 = CARTESIAN_POINT ( 'NONE',  ( 2.881552333950327061, 39.80724601559477094, 51.34430340187066122 ) ) ;
#18143 = EDGE_CURVE ( 'NONE', #2375, #7505, #16081, .T. ) ;
#18144 = CIRCLE ( 'NONE', #14821, 19.11328065563151668 ) ;
#18145 = LINE ( 'NONE', #16427, #11460 ) ;
#18146 = VECTOR ( 'NONE', #7853, 1000.000000000000000 ) ;
#18147 = CIRCLE ( 'NONE', #19596, 34.90673715956759082 ) ;
#18148 = EDGE_LOOP ( 'NONE', ( #18263, #13333, #8594, #3585 ) ) ;
#18149 = CARTESIAN_POINT ( 'NONE',  ( 44.60000000000000853, -9.600000000000001421, -47.50000000000000000 ) ) ;
#18150 = CARTESIAN_POINT ( 'NONE',  ( -10.49999999999980282, -2.516660498395515866, -105.0000000000000142 ) ) ;
#18151 = EDGE_CURVE ( 'NONE', #3077, #2472, #5474, .T. ) ;
#18152 = CIRCLE ( 'NONE', #577, 12.00000000000000355 ) ;
#18153 = DIRECTION ( 'NONE',  ( 0.000000000000000000, 0.000000000000000000, 1.000000000000000000 ) ) ;
#18154 = ADVANCED_FACE ( 'NONE', ( #18076 ), #14635, .T. ) ;
#18155 = ORIENTED_EDGE ( 'NONE', *, *, #9326, .T. ) ;
#18156 = ORIENTED_EDGE ( 'NONE', *, *, #18143, .T. ) ;
#18157 = EDGE_LOOP ( 'NONE', ( #10423, #4058, #14269, #20101 ) ) ;
#18158 = VECTOR ( 'NONE', #13008, 1000.000000000000000 ) ;
#18159 = AXIS2_PLACEMENT_3D ( 'NONE', #14162, #19574, #12675 ) ;
#18160 = VECTOR ( 'NONE', #3360, 1000.000000000000000 ) ;
#18161 = VERTEX_POINT ( 'NONE', #12683 ) ;
#18162 = DIRECTION ( 'NONE',  ( 1.296372316667914327E-16, 1.000000000000000000, -0.000000000000000000 ) ) ;
#18163 = DIRECTION ( 'NONE',  ( 0.000000000000000000, 1.000000000000000000, 0.000000000000000000 ) ) ;
#18164 = TOROIDAL_SURFACE ( 'NONE', #8641, 50.00000000000000000, 10.00000000000000000 ) ;
#18165 = FACE_OUTER_BOUND ( 'NONE', #12696, .T. ) ;
#18166 = ORIENTED_EDGE ( 'NONE', *, *, #1839, .T. ) ;
#18167 = DIRECTION ( 'NONE',  ( -0.000000000000000000, -1.000000000000000000, -0.000000000000000000 ) ) ;
#18168 = EDGE_CURVE ( 'NONE', #2517, #928, #21354, .T. ) ;
#18169 = AXIS2_PLACEMENT_3D ( 'NONE', #7895, #1017, #8017 ) ;
#18170 = ORIENTED_EDGE ( 'NONE', *, *, #17744, .T. ) ;
#18171 = CARTESIAN_POINT ( 'NONE',  ( 12.11890052765070713, 39.66666666666666430, -54.74394698394421965 ) ) ;
#18172 = CARTESIAN_POINT ( 'NONE',  ( 32.83234229683737482, -11.85401191286897316, -2.999999999999971578 ) ) ;
#18173 = CARTESIAN_POINT ( 'NONE',  ( 9.431193366787989042E-16, -3.025303850726725141, 0.000000000000000000 ) ) ;
#18174 = FACE_OUTER_BOUND ( 'NONE', #4970, .T. ) ;
#18175 = CARTESIAN_POINT ( 'NONE',  ( 22.97438720605776652, -22.98755168577443087, 2.999999999999995559 ) ) ;
#18176 = CARTESIAN_POINT ( 'NONE',  ( 42.50000000000000711, -12.00000000000012434, -50.02500000000011227 ) ) ;
#18177 = DIRECTION ( 'NONE',  ( -6.505213034913038160E-19, -3.903127820947822896E-18, -1.000000000000000000 ) ) ;
#18178 = ORIENTED_EDGE ( 'NONE', *, *, #5649, .T. ) ;
#18179 = CIRCLE ( 'NONE', #9017, 31.50000000000001421 ) ;
#18180 = VERTEX_POINT ( 'NONE', #14518 ) ;
#18181 = ORIENTED_EDGE ( 'NONE', *, *, #14188, .F. ) ;
#18182 = CARTESIAN_POINT ( 'NONE',  ( 10.39230484541330846, -25.00000000000000000, -5.999999999999929834 ) ) ;
#18183 = AXIS2_PLACEMENT_3D ( 'NONE', #5293, #15804, #6563 ) ;
#18184 = B_SPLINE_CURVE_WITH_KNOTS ( 'NONE', 3,
 ( #343, #5287, #16033, #17640, #1948, #6897 ),
 .UNSPECIFIED., .F., .F.,
 ( 4, 2, 4 ),
 ( 0.000000000000000000, 0.002641318319677492515, 0.005282636639354985029 ),
 .UNSPECIFIED. ) ;
#18185 = FACE_OUTER_BOUND ( 'NONE', #17208, .T. ) ;
#18186 = AXIS2_PLACEMENT_3D ( 'NONE', #5657, #2338, #14234 ) ;
#18187 = EDGE_CURVE ( 'NONE', #19656, #9609, #716, .T. ) ;
#18188 = CARTESIAN_POINT ( 'NONE',  ( 1.387778780781445676E-14, 40.00000000000000000, 48.73397172404482802 ) ) ;
#18189 = LINE ( 'NONE', #13234, #2888 ) ;
#18190 = DIRECTION ( 'NONE',  ( 0.000000000000000000, -1.000000000000000000, 0.000000000000000000 ) ) ;
#18191 = CARTESIAN_POINT ( 'NONE',  ( -34.99999999999999289, 5.000000000000000000, -9.000000000000065725 ) ) ;
#18192 = CARTESIAN_POINT ( 'NONE',  ( 35.00000000000000000, 17.00000000000000000, 2.365113165210053967E-14 ) ) ;
#18193 = CARTESIAN_POINT ( 'NONE',  ( 7.310544252644470693E-15, 28.19616000222403684, 0.000000000000000000 ) ) ;
#18194 = VERTEX_POINT ( 'NONE', #13138 ) ;
#18195 = DIRECTION ( 'NONE',  ( -0.000000000000000000, 1.000000000000000000, -0.000000000000000000 ) ) ;
#18196 = ADVANCED_FACE ( 'NONE', ( #21756 ), #17967, .F. ) ;
#18197 = CARTESIAN_POINT ( 'NONE',  ( -35.43002037646303393, 7.196011215416572959, -2.933296326616368521 ) ) ;
#18198 = DIRECTION ( 'NONE',  ( 1.000000000000000000, 0.000000000000000000, 0.000000000000000000 ) ) ;
#18199 = B_SPLINE_CURVE_WITH_KNOTS ( 'NONE', 3,
 ( #1057, #20193, #21804, #722, #11478, #21922 ),
 .UNSPECIFIED., .F., .F.,
 ( 4, 2, 4 ),
 ( 0.5000000000000000000, 0.7500000000000000000, 1.000000000000000000 ),
 .UNSPECIFIED. ) ;
#18200 = DIRECTION ( 'NONE',  ( 0.000000000000000000, 0.000000000000000000, -1.000000000000000000 ) ) ;
#18201 = ORIENTED_EDGE ( 'NONE', *, *, #17214, .T. ) ;
#18202 = CIRCLE ( 'NONE', #9419, 22.00000000000000000 ) ;
#18203 = ORIENTED_EDGE ( 'NONE', *, *, #22554, .T. ) ;
#18204 = DIRECTION ( 'NONE',  ( -0.000000000000000000, 1.000000000000000000, -0.000000000000000000 ) ) ;
#18205 = VECTOR ( 'NONE', #4250, 1000.000000000000000 ) ;
#18206 = DIRECTION ( 'NONE',  ( -6.505213034913038160E-19, -3.903127820947822896E-18, -1.000000000000000000 ) ) ;
#18207 = VECTOR ( 'NONE', #20392, 1000.000000000000000 ) ;
#18208 = ADVANCED_FACE ( 'NONE', ( #7427 ), #19706, .T. ) ;
#18209 = VERTEX_POINT ( 'NONE', #14738 ) ;
#18210 = CARTESIAN_POINT ( 'NONE',  ( 27.84804035626042662, -24.75236754129164751, 3.000000000000023537 ) ) ;
#18211 = EDGE_CURVE ( 'NONE', #18787, #11321, #3657, .T. ) ;
#18212 = AXIS2_PLACEMENT_3D ( 'NONE', #18127, #7702, #17668 ) ;
#18213 = CARTESIAN_POINT ( 'NONE',  ( 2.425343827396499563, 40.00000000000000000, -50.22135669491186150 ) ) ;
#18214 = EDGE_LOOP ( 'NONE', ( #9111, #3946 ) ) ;
#18215 = CARTESIAN_POINT ( 'NONE',  ( 1.814350108393116612, 39.98032087727209216, -50.09305062634004457 ) ) ;
#18216 = DIRECTION ( 'NONE',  ( 6.505213034913038160E-19, 3.903127820947822896E-18, 1.000000000000000000 ) ) ;
#18217 = CIRCLE ( 'NONE', #5437, 58.99999999999700862 ) ;
#18218 = VERTEX_POINT ( 'NONE', #21875 ) ;
#18219 = CARTESIAN_POINT ( 'NONE',  ( 2.775557561562891351E-14, -2.775557561562891351E-14, 2.999999999999995559 ) ) ;
#18220 = DIRECTION ( 'NONE',  ( 1.000000000000000000, 0.000000000000000000, 0.000000000000000000 ) ) ;
#18221 = FACE_OUTER_BOUND ( 'NONE', #20427, .T. ) ;
#18222 = AXIS2_PLACEMENT_3D ( 'NONE', #10259, #1114, #15063 ) ;
#18223 = CARTESIAN_POINT ( 'NONE',  ( -6.000000000000000888, -40.00000000000000000, -5.999999999999998224 ) ) ;
#18224 = DIRECTION ( 'NONE',  ( 0.000000000000000000, 0.000000000000000000, 1.000000000000000000 ) ) ;
#18225 = VERTEX_POINT ( 'NONE', #9599 ) ;
#18226 = CARTESIAN_POINT ( 'NONE',  ( 2.220446049250313081E-13, -2.498001805406602216E-13, -6.859353255829918616 ) ) ;
#18227 = FACE_BOUND ( 'NONE', #8152, .T. ) ;
#18228 = CARTESIAN_POINT ( 'NONE',  ( 13.33780792069982724, 2.142135623730938132, 45.06383732350703042 ) ) ;
#18229 = ORIENTED_EDGE ( 'NONE', *, *, #22331, .T. ) ;
#18230 = CONICAL_SURFACE ( 'NONE', #301, 34.00000000000000000, 1.308996938995746095 ) ;
#18231 = CARTESIAN_POINT ( 'NONE',  ( -4.074925817841607234, 32.10132595304121850, 3.000000000000016431 ) ) ;
#18232 = DIRECTION ( 'NONE',  ( 0.000000000000000000, 0.000000000000000000, -1.000000000000000000 ) ) ;
#18233 = EDGE_CURVE ( 'NONE', #6550, #7020, #6942, .T. ) ;
#18234 = AXIS2_PLACEMENT_3D ( 'NONE', #18845, #6697, #12185 ) ;
#18235 = AXIS2_PLACEMENT_3D ( 'NONE', #10342, #8527, #1660 ) ;
#18236 = AXIS2_PLACEMENT_3D ( 'NONE', #1909, #3749, #2019 ) ;
#18237 = VECTOR ( 'NONE', #19967, 1000.000000000000000 ) ;
#18238 = EDGE_LOOP ( 'NONE', ( #9202, #9748, #8550, #17950 ) ) ;
#18239 = ADVANCED_FACE ( 'NONE', ( #9386 ), #7887, .F. ) ;
#18240 = EDGE_LOOP ( 'NONE', ( #15542, #3106, #17726, #10475 ) ) ;
#18241 = ORIENTED_EDGE ( 'NONE', *, *, #8521, .T. ) ;
#18242 = DIRECTION ( 'NONE',  ( -0.9369493372187405189, -0.3494420069955173069, -0.004027807382165041368 ) ) ;
#18243 = ORIENTED_EDGE ( 'NONE', *, *, #5233, .F. ) ;
#18244 = CARTESIAN_POINT ( 'NONE',  ( 17.68684951551751539, 29.34943212427064196, -60.02035230153429524 ) ) ;
#18245 = CARTESIAN_POINT ( 'NONE',  ( 9.367793990832153028, -4.928932186883191235, 51.00106331757443456 ) ) ;
#18246 = LINE ( 'NONE', #7812, #4074 ) ;
#18247 = DIRECTION ( 'NONE',  ( 0.000000000000000000, 0.000000000000000000, -1.000000000000000000 ) ) ;
#18248 = DIRECTION ( 'NONE',  ( 0.000000000000000000, 0.000000000000000000, 1.000000000000000000 ) ) ;
#18249 = ORIENTED_EDGE ( 'NONE', *, *, #789, .F. ) ;
#18250 = DIRECTION ( 'NONE',  ( 0.000000000000000000, 0.000000000000000000, -1.000000000000000000 ) ) ;
#18251 = CARTESIAN_POINT ( 'NONE',  ( -5.999999999999998224, 20.00000000000000000, 5.999999999999999112 ) ) ;
#18252 = ORIENTED_EDGE ( 'NONE', *, *, #21735, .T. ) ;
#18253 = LINE ( 'NONE', #20200, #15624 ) ;
#18254 = CARTESIAN_POINT ( 'NONE',  ( -13.56354382738803999, 2.142135623730931471, -56.03997097393684612 ) ) ;
#18255 = CARTESIAN_POINT ( 'NONE',  ( 14.84934717125626946, 6.596698521592450071, -59.12425370493863142 ) ) ;
#18256 = ORIENTED_EDGE ( 'NONE', *, *, #10432, .T. ) ;
#18257 = CARTESIAN_POINT ( 'NONE',  ( -4.936596639065260916, -31.11077005834428277, -6.999999999999950262 ) ) ;
#18258 = EDGE_CURVE ( 'NONE', #18626, #10068, #12416, .T. ) ;
#18259 = DIRECTION ( 'NONE',  ( 1.000000000000000000, 1.208970125616063182E-17, 0.000000000000000000 ) ) ;
#18260 = ORIENTED_EDGE ( 'NONE', *, *, #19614, .F. ) ;
#18261 = CIRCLE ( 'NONE', #16029, 18.00000000000000355 ) ;
#18262 = CARTESIAN_POINT ( 'NONE',  ( -5.511187417680089240, 0.6970053750307799723, -52.42166665191985686 ) ) ;
#18263 = ORIENTED_EDGE ( 'NONE', *, *, #11917, .F. ) ;
#18264 = DIRECTION ( 'NONE',  ( 0.000000000000000000, -1.000000000000000000, 0.000000000000000000 ) ) ;
#18265 = CARTESIAN_POINT ( 'NONE',  ( -5.999999999999996447, 20.00000000000000000, 5.999999999999998224 ) ) ;
#18266 = EDGE_CURVE ( 'NONE', #11125, #19820, #16359, .T. ) ;
#18267 = CARTESIAN_POINT ( 'NONE',  ( 9.829668860674836139, 37.49547983896071912, -57.11616152308156558 ) ) ;
#18268 = AXIS2_PLACEMENT_3D ( 'NONE', #22553, #5019, #13924 ) ;
#18269 = AXIS2_PLACEMENT_3D ( 'NONE', #5642, #12616, #19631 ) ;
#18270 = ORIENTED_EDGE ( 'NONE', *, *, #8804, .T. ) ;
#18271 = ORIENTED_EDGE ( 'NONE', *, *, #4829, .T. ) ;
#18272 = ORIENTED_EDGE ( 'NONE', *, *, #5933, .T. ) ;
#18273 = AXIS2_PLACEMENT_3D ( 'NONE', #1648, #15491, #16993 ) ;
#18274 = ORIENTED_EDGE ( 'NONE', *, *, #16648, .T. ) ;
#18275 = CARTESIAN_POINT ( 'NONE',  ( -17.86915608785649567, 27.01645732367846620, -2.999999999999999112 ) ) ;
#18276 = CYLINDRICAL_SURFACE ( 'NONE', #3421, 19.11328065563151668 ) ;
#18277 = ORIENTED_EDGE ( 'NONE', *, *, #6377, .F. ) ;
#18278 = CARTESIAN_POINT ( 'NONE',  ( -2.836563456948004695E-15, -1.236374842841498678, -48.24164917503444627 ) ) ;
#18279 = VERTEX_POINT ( 'NONE', #11879 ) ;
#18280 = EDGE_CURVE ( 'NONE', #2957, #13632, #13354, .T. ) ;
#18281 = TOROIDAL_SURFACE ( 'NONE', #20478, 22.00000000000000000, 2.000000000000000000 ) ;
#18282 = EDGE_LOOP ( 'NONE', ( #7456, #1445, #20576, #3532 ) ) ;
#18283 = CARTESIAN_POINT ( 'NONE',  ( -16.99647590252643781, -30.48934413892778750, -2.999999999999992450 ) ) ;
#18284 = CARTESIAN_POINT ( 'NONE',  ( 3.266360431321861887E-15, -2.999999999999995559, 0.000000000000000000 ) ) ;
#18285 = DIRECTION ( 'NONE',  ( -0.000000000000000000, -1.000000000000000000, -0.000000000000000000 ) ) ;
#18286 = CARTESIAN_POINT ( 'NONE',  ( -90.00000000000000000, 24.73819270004212356, -9.108981535246192915E-16 ) ) ;
#18287 = EDGE_CURVE ( 'NONE', #13528, #13224, #8404, .T. ) ;
#18288 = EDGE_CURVE ( 'NONE', #1702, #9194, #18341, .T. ) ;
#18289 = ADVANCED_FACE ( 'NONE', ( #16927 ), #9835, .F. ) ;
#18290 = CARTESIAN_POINT ( 'NONE',  ( 5.551115123125782702E-14, -1.387778780781445676E-13, -5.749999999999949374 ) ) ;
#18291 = CARTESIAN_POINT ( 'NONE',  ( 4.044183821322609990E-15, 3.000000000000006217, 0.000000000000000000 ) ) ;
#18292 = CARTESIAN_POINT ( 'NONE',  ( 35.00000000000001421, 1.000000000000044187, -10.00000000000000000 ) ) ;
#18293 = ORIENTED_EDGE ( 'NONE', *, *, #2705, .T. ) ;
#18294 = ORIENTED_EDGE ( 'NONE', *, *, #7408, .F. ) ;
#18295 = AXIS2_PLACEMENT_3D ( 'NONE', #16105, #6030, #2250 ) ;
#18296 = VERTEX_POINT ( 'NONE', #1009 ) ;
#18297 = CARTESIAN_POINT ( 'NONE',  ( -21.29213537401196632, 12.67546417994314290, 58.41859095437464333 ) ) ;
#18298 = CARTESIAN_POINT ( 'NONE',  ( -35.00000000000000000, 40.00000000000000000, 1.387778780781445676E-14 ) ) ;
#18299 = FACE_BOUND ( 'NONE', #20213, .T. ) ;
#18300 = CARTESIAN_POINT ( 'NONE',  ( -0.2893420571180744250, -0.01224453477246341404, -48.63018218499168910 ) ) ;
#18301 = VECTOR ( 'NONE', #20462, 1000.000000000000000 ) ;
#18302 = FACE_OUTER_BOUND ( 'NONE', #4500, .T. ) ;
#18303 = LINE ( 'NONE', #17230, #16397 ) ;
#18304 = FACE_OUTER_BOUND ( 'NONE', #809, .T. ) ;
#18305 = CARTESIAN_POINT ( 'NONE',  ( -16.06969024216335740, -19.15111107797456924, -2.999999999999995559 ) ) ;
#18306 = CARTESIAN_POINT ( 'NONE',  ( 25.99999999999998579, 19.99999999999999645, 60.00099999999999767 ) ) ;
#18307 = DIRECTION ( 'NONE',  ( -0.000000000000000000, -1.000000000000000000, -0.000000000000000000 ) ) ;
#18308 = VERTEX_POINT ( 'NONE', #6506 ) ;
#18309 = DIRECTION ( 'NONE',  ( -1.000000000000000000, 0.000000000000000000, 0.000000000000000000 ) ) ;
#18310 = DIRECTION ( 'NONE',  ( 6.505213034913038160E-19, 3.903127820947822896E-18, 1.000000000000000000 ) ) ;
#18311 = CARTESIAN_POINT ( 'NONE',  ( 90.00000000000000000, 28.00000000000000000, -9.108981535246192915E-16 ) ) ;
#18312 = ORIENTED_EDGE ( 'NONE', *, *, #19505, .F. ) ;
#18313 = FACE_BOUND ( 'NONE', #13182, .T. ) ;
#18314 = ORIENTED_EDGE ( 'NONE', *, *, #19503, .F. ) ;
#18315 = CARTESIAN_POINT ( 'NONE',  ( 29.99999999999998579, 20.00000000000000711, 100.0000000000000000 ) ) ;
#18316 = CYLINDRICAL_SURFACE ( 'NONE', #4253, 2.099999999999997868 ) ;
#18317 = EDGE_CURVE ( 'NONE', #21371, #13393, #16462, .T. ) ;
#18318 = AXIS2_PLACEMENT_3D ( 'NONE', #11626, #6357, #18734 ) ;
#18319 = EDGE_CURVE ( 'NONE', #18025, #12070, #20379, .T. ) ;
#18320 = ORIENTED_EDGE ( 'NONE', *, *, #15041, .T. ) ;
#18321 = DIRECTION ( 'NONE',  ( -6.505213034913038160E-19, -3.903127820947822896E-18, -1.000000000000000000 ) ) ;
#18322 = EDGE_CURVE ( 'NONE', #13710, #16662, #4684, .T. ) ;
#18323 = CARTESIAN_POINT ( 'NONE',  ( 5.863462918964529536, 39.99999999999999289, -52.03112467568187327 ) ) ;
#18324 = ORIENTED_EDGE ( 'NONE', *, *, #12470, .T. ) ;
#18325 = CARTESIAN_POINT ( 'NONE',  ( 1.328666390486187066, 39.98974554208385968, -49.74045989696038816 ) ) ;
#18326 = FACE_OUTER_BOUND ( 'NONE', #8316, .T. ) ;
#18327 = CARTESIAN_POINT ( 'NONE',  ( 31.11077005834428277, -4.936596639065260916, -2.999999999999971578 ) ) ;
#18328 = CARTESIAN_POINT ( 'NONE',  ( -3.092934392865752891, 39.99999999999999289, 50.60141176657413098 ) ) ;
#18329 = CARTESIAN_POINT ( 'NONE',  ( 10.71765026523584829, 39.18334136350156882, -54.91251049708800025 ) ) ;
#18330 = DIRECTION ( 'NONE',  ( -0.000000000000000000, -1.000000000000000000, -0.000000000000000000 ) ) ;
#18331 = CIRCLE ( 'NONE', #17956, 2.524999999999999467 ) ;
#18332 = DIRECTION ( 'NONE',  ( 0.000000000000000000, 1.000000000000000000, 0.000000000000000000 ) ) ;
#18333 = VERTEX_POINT ( 'NONE', #22333 ) ;
#18334 = CARTESIAN_POINT ( 'NONE',  ( 7.196011215416979745, 35.43002037646296998, -2.933296326616370298 ) ) ;
#18335 = DIRECTION ( 'NONE',  ( 0.000000000000000000, 1.000000000000000000, 0.000000000000000000 ) ) ;
#18336 = CARTESIAN_POINT ( 'NONE',  ( -0.01944734386466554985, 39.99999780157233431, -48.74910573947852299 ) ) ;
#18337 = ORIENTED_EDGE ( 'NONE', *, *, #15990, .F. ) ;
#18338 = EDGE_CURVE ( 'NONE', #13199, #3604, #11546, .T. ) ;
#18339 = DIRECTION ( 'NONE',  ( 6.505213034913038160E-19, 3.903127820947822896E-18, 1.000000000000000000 ) ) ;
#18340 = CARTESIAN_POINT ( 'NONE',  ( -21.69517388068220853, -28.13960001536977629, -2.999999999999998224 ) ) ;
#18341 = B_SPLINE_CURVE_WITH_KNOTS ( 'NONE', 3,
 ( #8010, #18764, #1227, #15187, #16824, #21990, #8224, #20265, #22436, #13472, #6282, #10040, #22212 ),
 .UNSPECIFIED., .F., .F.,
 ( 4, 2, 1, 1, 1, 2, 2, 4 ),
 ( 0.000000000000000000, 0.2499999999999900080, 0.3749999999999875100, 0.4374999999999895084, 0.4687499999999898415, 0.4843749999999922839, 0.4999999999999947820, 1.000000000000000000 ),
 .UNSPECIFIED. ) ;
#18342 = ORIENTED_EDGE ( 'NONE', *, *, #5667, .F. ) ;
#18343 = ORIENTED_EDGE ( 'NONE', *, *, #18998, .T. ) ;
#18344 = ORIENTED_EDGE ( 'NONE', *, *, #22440, .F. ) ;
#18345 = CARTESIAN_POINT ( 'NONE',  ( 11.03199507241028066, 39.99999999999999289, 53.98106524768372338 ) ) ;
#18346 = CARTESIAN_POINT ( 'NONE',  ( -35.00000000000000000, -4.928932188134504955, 1.387778780781445676E-14 ) ) ;
#18347 = DIRECTION ( 'NONE',  ( 6.505213034913038160E-19, 3.903127820947822896E-18, 1.000000000000000000 ) ) ;
#18348 = DIRECTION ( 'NONE',  ( -0.000000000000000000, -1.000000000000000000, -0.000000000000000000 ) ) ;
#18349 = CARTESIAN_POINT ( 'NONE',  ( 2.090752864397209532, 5.144172964797016689, -38.95144853163193943 ) ) ;
#18350 = EDGE_LOOP ( 'NONE', ( #11137, #34, #11801, #11937 ) ) ;
#18351 = LINE ( 'NONE', #1278, #336 ) ;
#18352 = CARTESIAN_POINT ( 'NONE',  ( -34.99999999999999289, -3.999999999999985345, -3.012171160963566127E-14 ) ) ;
#18353 = VERTEX_POINT ( 'NONE', #18539 ) ;
#18354 = CARTESIAN_POINT ( 'NONE',  ( -5.833333333333337478, 6.180730040185833829, -40.61164310337066041 ) ) ;
#18355 = EDGE_CURVE ( 'NONE', #16393, #21378, #10155, .T. ) ;
#18356 = CARTESIAN_POINT ( 'NONE',  ( 90.00000000000000000, 39.97500000000000142, -9.108981535246192915E-16 ) ) ;
#18357 = AXIS2_PLACEMENT_3D ( 'NONE', #21230, #4052, #14443 ) ;
#18358 = DIRECTION ( 'NONE',  ( 0.000000000000000000, 0.000000000000000000, 1.000000000000000000 ) ) ;
#18359 = ORIENTED_EDGE ( 'NONE', *, *, #1012, .T. ) ;
#18360 = CARTESIAN_POINT ( 'NONE',  ( 35.00000000000000000, 0.000000000000000000, 54.99999999999698019 ) ) ;
#18361 = CARTESIAN_POINT ( 'NONE',  ( 5.302679949206165588, 39.28774282260669537, -54.25155191766006624 ) ) ;
#18362 = ORIENTED_EDGE ( 'NONE', *, *, #21365, .F. ) ;
#18363 = DIRECTION ( 'NONE',  ( 0.000000000000000000, -0.5150380749100547106, -0.8571673007021120005 ) ) ;
#18364 = CARTESIAN_POINT ( 'NONE',  ( -7.505578006075234399, 1.461761173328252950, -55.63523492904088386 ) ) ;
#18365 = EDGE_CURVE ( 'NONE', #16838, #6573, #17033, .T. ) ;
#18366 = ORIENTED_EDGE ( 'NONE', *, *, #7625, .F. ) ;
#18367 = EDGE_CURVE ( 'NONE', #15787, #12263, #21223, .T. ) ;
#18368 = UNCERTAINTY_MEASURE_WITH_UNIT (LENGTH_MEASURE( 1.000000000000000082E-05 ), #1763, 'distance_accuracy_value', 'NONE');
#18369 = FACE_BOUND ( 'NONE', #21654, .T. ) ;
#18370 = CARTESIAN_POINT ( 'NONE',  ( -15.00000000000001421, 20.00000000000000355, -105.0020000000000095 ) ) ;
#18371 = DIRECTION ( 'NONE',  ( 0.000000000000000000, 1.000000000000000000, 0.000000000000000000 ) ) ;
#18372 = CARTESIAN_POINT ( 'NONE',  ( 19.81218727895565124, 22.86772234701075490, -58.09777938302214295 ) ) ;
#18373 = VERTEX_POINT ( 'NONE', #2964 ) ;
#18374 = AXIS2_PLACEMENT_3D ( 'NONE', #4137, #3916, #16042 ) ;
#18375 = EDGE_LOOP ( 'NONE', ( #15601, #5258, #4940, #21332 ) ) ;
#18376 = EDGE_CURVE ( 'NONE', #11307, #4097, #17149, .T. ) ;
#18377 = ORIENTED_EDGE ( 'NONE', *, *, #2889, .F. ) ;
#18378 = ORIENTED_EDGE ( 'NONE', *, *, #3000, .T. ) ;
#18379 = CARTESIAN_POINT ( 'NONE',  ( 26.10603996529656357, 24.10117729468382564, 3.000000000000030198 ) ) ;
#18380 = DIRECTION ( 'NONE',  ( -1.000000000000000000, 0.000000000000000000, 0.000000000000000000 ) ) ;
#18381 = EDGE_LOOP ( 'NONE', ( #3445, #4930, #7258, #9409 ) ) ;
#18382 = CARTESIAN_POINT ( 'NONE',  ( -29.32895111104219410, -20.05817253550624812, -2.999999999999996447 ) ) ;
#18383 = CARTESIAN_POINT ( 'NONE',  ( 1.845281852387030908, 13.60278332471100704, 6.813359845936179049 ) ) ;
#18384 = ORIENTED_EDGE ( 'NONE', *, *, #17291, .T. ) ;
#18385 = EDGE_CURVE ( 'NONE', #20079, #13970, #11697, .T. ) ;
#18386 = LINE ( 'NONE', #13439, #18301 ) ;
#18387 = CARTESIAN_POINT ( 'NONE',  ( 32.20238537491839992, 4.080045426412798548, -6.999999999999950262 ) ) ;
#18388 = CARTESIAN_POINT ( 'NONE',  ( 42.50000000000000000, 10.00000000000000000, 47.49999999999999289 ) ) ;
#18389 = CARTESIAN_POINT ( 'NONE',  ( 35.00000000000001421, -5.000000000000000000, -4.999999999999997335 ) ) ;
#18390 = CARTESIAN_POINT ( 'NONE',  ( 20.17230487860829768, 25.34312177887326811, -2.999999999999971578 ) ) ;
#18391 = VECTOR ( 'NONE', #22230, 1000.000000000000000 ) ;
#18392 = AXIS2_PLACEMENT_3D ( 'NONE', #4190, #19776, #18038 ) ;
#18393 = AXIS2_PLACEMENT_3D ( 'NONE', #10468, #20921, #18975 ) ;
#18394 = LINE ( 'NONE', #2715, #9298 ) ;
#18395 = CARTESIAN_POINT ( 'NONE',  ( -89.99999999999701572, 0.000000000000000000, -2.500000000000038636 ) ) ;
#18396 = ORIENTED_EDGE ( 'NONE', *, *, #22395, .F. ) ;
#18397 = ORIENTED_EDGE ( 'NONE', *, *, #3662, .F. ) ;
#18398 = EDGE_CURVE ( 'NONE', #1157, #21604, #14618, .T. ) ;
#18399 = VERTEX_POINT ( 'NONE', #13695 ) ;
#18400 = CARTESIAN_POINT ( 'NONE',  ( -17.41694144196565119, 10.15895996405112456, 59.94253659024146685 ) ) ;
#18401 = DIRECTION ( 'NONE',  ( 6.505213034913038160E-19, 3.903127820947822896E-18, 1.000000000000000000 ) ) ;
#18402 = AXIS2_PLACEMENT_3D ( 'NONE', #15976, #11986, #12320 ) ;
#18403 = VECTOR ( 'NONE', #16185, 1000.000000000000000 ) ;
#18404 = CARTESIAN_POINT ( 'NONE',  ( -6.000000000000000000, 20.00000000000000000, -5.999999999999999112 ) ) ;
#18405 = CARTESIAN_POINT ( 'NONE',  ( 0.4211638912362005716, -0.02267170258719574880, -49.14966933624602774 ) ) ;
#18406 = EDGE_CURVE ( 'NONE', #7389, #10163, #3596, .T. ) ;
#18407 = CONICAL_SURFACE ( 'NONE', #1940, 8.999999999999973355, 0.7853981633974657095 ) ;
#18408 = CARTESIAN_POINT ( 'NONE',  ( -30.13956425491219449, -21.05198877411826430, 2.800654218530505890 ) ) ;
#18409 = CARTESIAN_POINT ( 'NONE',  ( 1.591932335265033587E-15, -4.923002280079127832E-27, 50.50395615645412306 ) ) ;
#18410 = CARTESIAN_POINT ( 'NONE',  ( 9.689843208404433028, 39.33333333333334991, 54.54983754392749518 ) ) ;
#18411 = CARTESIAN_POINT ( 'NONE',  ( -5.340789179572220213, 39.27722415257183286, -54.28402915905239468 ) ) ;
#18412 = CARTESIAN_POINT ( 'NONE',  ( -42.50000000000000711, -12.00000000000012434, 47.50000000000000711 ) ) ;
#18413 = VERTEX_POINT ( 'NONE', #17373 ) ;
#18414 = CARTESIAN_POINT ( 'NONE',  ( -8.485281374238484275, 2.999999999999780620, -4.999999999999997335 ) ) ;
#18415 = EDGE_CURVE ( 'NONE', #17133, #5664, #20867, .T. ) ;
#18416 = CARTESIAN_POINT ( 'NONE',  ( -0.6237373291637031691, 39.99088417130654705, -49.47180386667445617 ) ) ;
#18417 = DIRECTION ( 'NONE',  ( -1.296372316667914327E-16, -1.000000000000000000, 0.000000000000000000 ) ) ;
#18418 = CARTESIAN_POINT ( 'NONE',  ( -35.00000000000000000, 22.00000000000000355, 2.365113165210053967E-14 ) ) ;
#18419 = ADVANCED_FACE ( 'NONE', ( #302 ), #6967, .F. ) ;
#18420 = ORIENTED_EDGE ( 'NONE', *, *, #15483, .F. ) ;
#18421 = DIRECTION ( 'NONE',  ( 0.000000000000000000, 0.000000000000000000, -1.000000000000000000 ) ) ;
#18422 = ORIENTED_EDGE ( 'NONE', *, *, #3927, .F. ) ;
#18423 = DIRECTION ( 'NONE',  ( -0.000000000000000000, -1.000000000000000000, -0.000000000000000000 ) ) ;
#18424 = CARTESIAN_POINT ( 'NONE',  ( 11.93972437435558653, 29.14949368109881433, -2.999999999999999112 ) ) ;
#18425 = AXIS2_PLACEMENT_3D ( 'NONE', #21411, #332, #14403 ) ;
#18426 = EDGE_CURVE ( 'NONE', #19936, #9264, #17606, .T. ) ;
#18427 = AXIS2_PLACEMENT_3D ( 'NONE', #15686, #17288, #15341 ) ;
#18428 = EDGE_CURVE ( 'NONE', #7580, #11124, #9148, .T. ) ;
#18429 = EDGE_LOOP ( 'NONE', ( #8262, #8929 ) ) ;
#18430 = CARTESIAN_POINT ( 'NONE',  ( 21.99999999999998579, 20.00000000000000355, -98.00000000000000000 ) ) ;
#18431 = CIRCLE ( 'NONE', #17745, 30.00000000000000000 ) ;
#18432 = MANIFOLD_SOLID_BREP ( 'Cut-Extrude3', #2377 ) ;
#18433 = CYLINDRICAL_SURFACE ( 'NONE', #16735, 0.9999999999999956701 ) ;
#18434 = ORIENTED_EDGE ( 'NONE', *, *, #12124, .T. ) ;
#18435 = CARTESIAN_POINT ( 'NONE',  ( 6.745307376263603771, 39.70676877995263965, -53.21562790720045655 ) ) ;
#18436 = CYLINDRICAL_SURFACE ( 'NONE', #746, 19.11328065563150957 ) ;
#18437 = AXIS2_PLACEMENT_3D ( 'NONE', #20162, #11336, #18089 ) ;
#18438 = CARTESIAN_POINT ( 'NONE',  ( 14.74639653023226948, -28.96193690644938101, 2.999999999999995559 ) ) ;
#18439 = CARTESIAN_POINT ( 'NONE',  ( 42.49999999999998579, 7.000000000000000000, -47.49999999999997868 ) ) ;
#18440 = CARTESIAN_POINT ( 'NONE',  ( 10.48823472801903200, 39.21814192261259535, -54.82890001962670112 ) ) ;
#18441 = AXIS2_PLACEMENT_3D ( 'NONE', #13263, #6418, #8247 ) ;
#18442 = EDGE_CURVE ( 'NONE', #20626, #12113, #6236, .T. ) ;
#18443 = CARTESIAN_POINT ( 'NONE',  ( 29.36548507648054240, 13.83143812983103693, -6.999999999999950262 ) ) ;
#18444 = EDGE_CURVE ( 'NONE', #5849, #16284, #21976, .T. ) ;
#18445 = DIRECTION ( 'NONE',  ( -6.505213034913038160E-19, -3.903127820947822896E-18, -1.000000000000000000 ) ) ;
#18446 = EDGE_LOOP ( 'NONE', ( #3029, #14927, #10235, #11984 ) ) ;
#18447 = DIRECTION ( 'NONE',  ( -1.000000000000000000, 0.000000000000000000, 0.000000000000000000 ) ) ;
#18448 = CARTESIAN_POINT ( 'NONE',  ( -34.99999999999999289, 38.99999999999999289, 60.00000000000001421 ) ) ;
#18449 = CARTESIAN_POINT ( 'NONE',  ( 35.00000000000001421, 0.000000000000000000, 1.540743955509788682E-30 ) ) ;
#18450 = FACE_OUTER_BOUND ( 'NONE', #11871, .T. ) ;
#18451 = VERTEX_POINT ( 'NONE', #2022 ) ;
#18452 = ADVANCED_FACE ( 'NONE', ( #21276, #12547 ), #3310, .T. ) ;
#18453 = VECTOR ( 'NONE', #12480, 1000.000000000000000 ) ;
#18454 = CARTESIAN_POINT ( 'NONE',  ( -16.66666666666666785, 20.00000000000000000, -23.57022603955158502 ) ) ;
#18455 = CARTESIAN_POINT ( 'NONE',  ( -42.50000000000000711, -11.97499999999999964, -50.00000000000000000 ) ) ;
#18456 = VECTOR ( 'NONE', #13754, 1000.000000000000000 ) ;
#18457 = VERTEX_POINT ( 'NONE', #644 ) ;
#18458 = ORIENTED_EDGE ( 'NONE', *, *, #21645, .F. ) ;
#18459 =( NAMED_UNIT ( * ) PLANE_ANGLE_UNIT ( ) SI_UNIT ( $, .RADIAN. ) );
#18460 = EDGE_LOOP ( 'NONE', ( #16307, #14711, #12050 ) ) ;
#18461 = CARTESIAN_POINT ( 'NONE',  ( 8.331955809010601399, 38.18181818181818699, 56.36098470834073026 ) ) ;
#18462 = CARTESIAN_POINT ( 'NONE',  ( 19.99999999999999645, -1.500000000000014433, 2.449293598294705724E-15 ) ) ;
#18463 = DIRECTION ( 'NONE',  ( 0.000000000000000000, 1.000000000000000000, 0.000000000000000000 ) ) ;
#18464 = CARTESIAN_POINT ( 'NONE',  ( -6.000000000000000000, 20.00000000000000000, -5.999999999999999112 ) ) ;
#18465 = CIRCLE ( 'NONE', #173, 31.50000000000001421 ) ;
#18466 = CARTESIAN_POINT ( 'NONE',  ( 35.00000000000058265, 26.00000000000000355, -55.00000000000076028 ) ) ;
#18467 = ORIENTED_EDGE ( 'NONE', *, *, #22658, .T. ) ;
#18468 = DIRECTION ( 'NONE',  ( -0.000000000000000000, -1.000000000000000000, -0.000000000000000000 ) ) ;
#18469 = FACE_OUTER_BOUND ( 'NONE', #13268, .T. ) ;
#18470 = ORIENTED_EDGE ( 'NONE', *, *, #16117, .T. ) ;
#18471 = CARTESIAN_POINT ( 'NONE',  ( -14.69988787053504531, 16.91499873015103006, -45.69379240540676790 ) ) ;
#18472 = EDGE_CURVE ( 'NONE', #10163, #21119, #10829, .T. ) ;
#18473 = CARTESIAN_POINT ( 'NONE',  ( -21.80163436544122746, 14.71892543950344923, -58.53048140122280074 ) ) ;
#18474 = B_SPLINE_CURVE_WITH_KNOTS ( 'NONE', 3,
 ( #3222, #6543, #17068, #10071 ),
 .UNSPECIFIED., .F., .F.,
 ( 4, 4 ),
 ( 0.001875451646902768750, 0.003761979286331133213 ),
 .UNSPECIFIED. ) ;
#18475 = CIRCLE ( 'NONE', #19929, 2.500000000000002220 ) ;
#18476 = DIRECTION ( 'NONE',  ( 0.000000000000000000, 0.000000000000000000, 1.000000000000000000 ) ) ;
#18477 = CARTESIAN_POINT ( 'NONE',  ( 19.95262135541528892, 18.40707545474674589, -60.61067493606136480 ) ) ;
#18478 = ORIENTED_EDGE ( 'NONE', *, *, #14749, .F. ) ;
#18479 = CARTESIAN_POINT ( 'NONE',  ( -2.774848922471319757, 40.00000000000000000, -50.42374039355618009 ) ) ;
#18480 = CARTESIAN_POINT ( 'NONE',  ( -14.76298474240489433, -28.95348479018577947, -6.999999999999999112 ) ) ;
#18481 = EDGE_LOOP ( 'NONE', ( #2269, #17474, #2439, #17325 ) ) ;
#18482 = CARTESIAN_POINT ( 'NONE',  ( 42.49999999999998579, 7.000000000000000000, -47.49999999999997868 ) ) ;
#18483 = VERTEX_POINT ( 'NONE', #19559 ) ;
#18484 = EDGE_CURVE ( 'NONE', #18822, #586, #363, .T. ) ;
#18485 = CARTESIAN_POINT ( 'NONE',  ( 3.330669073875469621E-13, -1.110223024625156540E-13, -2.999999999999971578 ) ) ;
#18486 = CYLINDRICAL_SURFACE ( 'NONE', #20987, 2.499999999999995115 ) ;
#18487 = AXIS2_PLACEMENT_3D ( 'NONE', #4226, #2166, #14402 ) ;
#18488 = AXIS2_PLACEMENT_3D ( 'NONE', #12026, #13941, #12133 ) ;
#18489 = CARTESIAN_POINT ( 'NONE',  ( 15.99370094303709955, 7.960486082689420151, -59.50964696496923523 ) ) ;
#18491 = VERTEX_POINT ( 'NONE', #19894 ) ;
#18490 = EDGE_CURVE ( 'NONE', #12877, #18279, #17244, .T. ) ;
#18492 = AXIS2_PLACEMENT_3D ( 'NONE', #17545, #19161, #20765 ) ;
#18493 = ORIENTED_EDGE ( 'NONE', *, *, #14410, .T. ) ;
#18494 = ORIENTED_EDGE ( 'NONE', *, *, #4711, .T. ) ;
#18495 = VERTEX_POINT ( 'NONE', #18052 ) ;
#18496 = CARTESIAN_POINT ( 'NONE',  ( 2.220446049250313081E-13, -8.326672684688674053E-14, 2.800654218530498785 ) ) ;
#18497 = DIRECTION ( 'NONE',  ( 0.000000000000000000, 1.000000000000000000, 0.000000000000000000 ) ) ;
#18498 = EDGE_CURVE ( 'NONE', #18984, #19146, #10954, .T. ) ;
#18499 = VERTEX_POINT ( 'NONE', #14717 ) ;
#18500 = CARTESIAN_POINT ( 'NONE',  ( 2.775557561562891351E-14, -2.775557561562891351E-14, 2.999999999999999112 ) ) ;
#18501 = CARTESIAN_POINT ( 'NONE',  ( -8.523345606559670884, -2.856915207742760199, -52.89411661591344682 ) ) ;
#18502 = ORIENTED_EDGE ( 'NONE', *, *, #12241, .T. ) ;
#18503 = AXIS2_PLACEMENT_3D ( 'NONE', #2992, #1378, #13607 ) ;
#18504 = CARTESIAN_POINT ( 'NONE',  ( -29.14949368109887118, 11.93972437435536449, -6.999999999999999112 ) ) ;
#18505 = CIRCLE ( 'NONE', #21823, 51.00000000000001421 ) ;
#18506 = ORIENTED_EDGE ( 'NONE', *, *, #8327, .F. ) ;
#18507 = DIRECTION ( 'NONE',  ( -6.505213034913038160E-19, -3.903127820947822896E-18, -1.000000000000000000 ) ) ;
#18508 = CONICAL_SURFACE ( 'NONE', #5696, 4.025000000000000355, 0.7853981633974136400 ) ;
#18509 = LINE ( 'NONE', #21497, #12726 ) ;
#18510 = DIRECTION ( 'NONE',  ( 6.505213034913038160E-19, 3.903127820947822896E-18, 1.000000000000000000 ) ) ;
#18511 = DIRECTION ( 'NONE',  ( -6.505213034913038160E-19, -3.903127820947822896E-18, -1.000000000000000000 ) ) ;
#18512 = CIRCLE ( 'NONE', #11557, 28.00000000000001066 ) ;
#18513 = CARTESIAN_POINT ( 'NONE',  ( -1.387778780781445518E-14, 20.00000000000000355, 100.0000000000000000 ) ) ;
#18514 = CONICAL_SURFACE ( 'NONE', #15949, 17.00000000000000355, 0.7853981633974539411 ) ;
#18515 = EDGE_CURVE ( 'NONE', #7324, #12042, #19790, .T. ) ;
#18516 = AXIS2_PLACEMENT_3D ( 'NONE', #408, #7400, #12774 ) ;
#18517 = ORIENTED_EDGE ( 'NONE', *, *, #22265, .F. ) ;
#18518 = CIRCLE ( 'NONE', #17799, 57.00000000000002132 ) ;
#18519 = VERTEX_POINT ( 'NONE', #19677 ) ;
#18520 = ORIENTED_EDGE ( 'NONE', *, *, #20260, .T. ) ;
#18521 = CARTESIAN_POINT ( 'NONE',  ( -16.72418712225133675, 8.992692292682194832, 57.18730031742740749 ) ) ;
#18522 = EDGE_CURVE ( 'NONE', #12474, #20078, #17555, .T. ) ;
#18523 = AXIS2_PLACEMENT_3D ( 'NONE', #18665, #8124, #15081 ) ;
#18524 = CARTESIAN_POINT ( 'NONE',  ( 1.110223024625156540E-13, -5.551115123125782702E-14, -6.999999999999950262 ) ) ;
#18525 = DIRECTION ( 'NONE',  ( 6.505213034913038160E-19, 3.903127820947822896E-18, 1.000000000000000000 ) ) ;
#18526 = CARTESIAN_POINT ( 'NONE',  ( -11.12223430625391707, 40.00000000000000711, 54.01173000072970609 ) ) ;
#18527 = CARTESIAN_POINT ( 'NONE',  ( -40.40000000000001279, -9.600000000000001421, 47.50000000000000711 ) ) ;
#18528 = ORIENTED_EDGE ( 'NONE', *, *, #11274, .F. ) ;
#18529 = CARTESIAN_POINT ( 'NONE',  ( -35.00000000000000000, 40.00000000000000000, 1.387778780781445676E-14 ) ) ;
#18530 = DIRECTION ( 'NONE',  ( 1.000000000000000000, 1.208970125616063182E-17, 0.000000000000000000 ) ) ;
#18531 = CYLINDRICAL_SURFACE ( 'NONE', #1048, 31.50000000000000711 ) ;
#18532 = AXIS2_PLACEMENT_3D ( 'NONE', #16816, #15070, #9827 ) ;
#18533 = CARTESIAN_POINT ( 'NONE',  ( 1.583519045122365076, -4.618580011808620434, 46.65783332780151227 ) ) ;
#18534 = DIRECTION ( 'NONE',  ( 0.000000000000000000, -0.7071067811865500152, -0.7071067811865450192 ) ) ;
#18535 = AXIS2_PLACEMENT_3D ( 'NONE', #5189, #8945, #3698 ) ;
#18536 = ADVANCED_FACE ( 'NONE', ( #17945 ), #7405, .F. ) ;
#18537 = EDGE_LOOP ( 'NONE', ( #18377, #35, #5006, #8330 ) ) ;
#18538 = FACE_OUTER_BOUND ( 'NONE', #14684, .T. ) ;
#18539 = CARTESIAN_POINT ( 'NONE',  ( -42.50000000000000711, -3.738192700042122674, -47.50000000000000000 ) ) ;
#18540 = DIRECTION ( 'NONE',  ( -0.000000000000000000, -1.000000000000000000, -0.000000000000000000 ) ) ;
#18541 = LINE ( 'NONE', #11327, #2343 ) ;
#18542 = VECTOR ( 'NONE', #10607, 1000.000000000000000 ) ;
#18543 = ORIENTED_EDGE ( 'NONE', *, *, #21013, .T. ) ;
#18544 = CARTESIAN_POINT ( 'NONE',  ( 35.00000000000000000, 39.00000000000000711, 4.258610482196280173E-15 ) ) ;
#18545 = FACE_OUTER_BOUND ( 'NONE', #13388, .T. ) ;
#18546 = DIRECTION ( 'NONE',  ( -1.000000000000000000, 0.000000000000000000, 0.000000000000000000 ) ) ;
#18547 = CARTESIAN_POINT ( 'NONE',  ( 4.724946350300523916E-15, 8.251288694035745053, 0.000000000000000000 ) ) ;
#18548 = EDGE_CURVE ( 'NONE', #7324, #17762, #2198, .T. ) ;
#18549 = EDGE_CURVE ( 'NONE', #6464, #19292, #6954, .T. ) ;
#18550 = TOROIDAL_SURFACE ( 'NONE', #20389, 18.00000000000000355, 4.000000000000000000 ) ;
#18551 = FACE_OUTER_BOUND ( 'NONE', #3277, .T. ) ;
#18552 = DIRECTION ( 'NONE',  ( 1.000000000000000000, 0.000000000000000000, 0.000000000000000000 ) ) ;
#18553 = ORIENTED_EDGE ( 'NONE', *, *, #4266, .T. ) ;
#18554 = DIRECTION ( 'NONE',  ( 0.000000000000000000, -1.000000000000000000, 0.000000000000000000 ) ) ;
#18555 = CARTESIAN_POINT ( 'NONE',  ( 35.00000000000000000, 17.00000000000000000, -40.99999999999997868 ) ) ;
#18556 = EDGE_CURVE ( 'NONE', #10193, #1471, #20135, .T. ) ;
#18557 = DIRECTION ( 'NONE',  ( -0.000000000000000000, 1.000000000000000000, -0.000000000000000000 ) ) ;
#18558 = CARTESIAN_POINT ( 'NONE',  ( 10.64189282826238170, 39.19489805863617704, -54.88474174631790703 ) ) ;
#18559 = CARTESIAN_POINT ( 'NONE',  ( -8.199064559763622029, 32.63945871574319568, -42.22991907770641262 ) ) ;
#18560 = CIRCLE ( 'NONE', #1014, 15.99999999999993072 ) ;
#18561 = CARTESIAN_POINT ( 'NONE',  ( -15.50000000000011013, 42.51666049839536043, -100.0000000000000000 ) ) ;
#18562 = EDGE_CURVE ( 'NONE', #9647, #6470, #3314, .T. ) ;
#18563 = EDGE_LOOP ( 'NONE', ( #22305, #3010, #2674, #11907 ) ) ;
#18564 = DIRECTION ( 'NONE',  ( -1.000000000000000000, 0.000000000000000000, 0.000000000000000000 ) ) ;
#18565 = VECTOR ( 'NONE', #17307, 1000.000000000000000 ) ;
#18566 = LINE ( 'NONE', #9860, #14034 ) ;
#18567 = CARTESIAN_POINT ( 'NONE',  ( 12.27586057105627582, 4.193657236093733864, -55.54740530681009858 ) ) ;
#18568 = CARTESIAN_POINT ( 'NONE',  ( -34.99999999999999289, 39.00000000000000711, 50.00000000000000000 ) ) ;
#18569 = AXIS2_PLACEMENT_3D ( 'NONE', #11891, #22113, #3203 ) ;
#18570 = ORIENTED_EDGE ( 'NONE', *, *, #22016, .T. ) ;
#18571 = CARTESIAN_POINT ( 'NONE',  ( 42.50000000000000711, -12.00000000000000000, -50.00000000000000000 ) ) ;
#18572 = CARTESIAN_POINT ( 'NONE',  ( -4.170748987303213084, 34.65667543218822999, -2.999999999999971578 ) ) ;
#18573 = EDGE_CURVE ( 'NONE', #3830, #4700, #763, .T. ) ;
#18574 = EDGE_CURVE ( 'NONE', #13854, #18007, #742, .T. ) ;
#18575 = EDGE_CURVE ( 'NONE', #7962, #15903, #14612, .T. ) ;
#18576 = AXIS2_PLACEMENT_3D ( 'NONE', #5982, #16289, #2441 ) ;
#18578 = EDGE_CURVE ( 'NONE', #7926, #3138, #12337, .T. ) ;
#18577 = ORIENTED_EDGE ( 'NONE', *, *, #16608, .F. ) ;
#18579 = AXIS2_PLACEMENT_3D ( 'NONE', #8054, #17082, #18593 ) ;
#18580 = AXIS2_PLACEMENT_3D ( 'NONE', #20398, #19941, #14764 ) ;
#18581 = EDGE_CURVE ( 'NONE', #15288, #13346, #1830, .T. ) ;
#18582 = ORIENTED_EDGE ( 'NONE', *, *, #6998, .T. ) ;
#18583 = DIRECTION ( 'NONE',  ( 0.1436291612043019972, 0.9896287191852406462, 0.002379541033241260213 ) ) ;
#18584 = CIRCLE ( 'NONE', #19688, 2.500000000000002220 ) ;
#18585 = ORIENTED_EDGE ( 'NONE', *, *, #20237, .F. ) ;
#18586 = CARTESIAN_POINT ( 'NONE',  ( 11.50056215611667554, 36.46966885432792083, -57.85578624339546394 ) ) ;
#18587 = DIRECTION ( 'NONE',  ( -1.000000000000000000, -1.208970125616077665E-17, 0.000000000000000000 ) ) ;
#18588 = LINE ( 'NONE', #19149, #406 ) ;
#18589 = CARTESIAN_POINT ( 'NONE',  ( 16.30820259622263890, 8.415540886845231938, 59.60694662124535625 ) ) ;
#18590 = DIRECTION ( 'NONE',  ( 0.000000000000000000, 0.000000000000000000, -1.000000000000000000 ) ) ;
#18591 = EDGE_LOOP ( 'NONE', ( #5032, #15678 ) ) ;
#18592 = DIRECTION ( 'NONE',  ( -6.505213034913038160E-19, -3.903127820947822896E-18, -1.000000000000000000 ) ) ;
#18593 = DIRECTION ( 'NONE',  ( 1.000000000000000000, 0.000000000000000000, 0.000000000000000000 ) ) ;
#18594 = ORIENTED_EDGE ( 'NONE', *, *, #5963, .F. ) ;
#18595 = CARTESIAN_POINT ( 'NONE',  ( 13.00000000000000178, 20.00000000000000000, -11.32475165290605901 ) ) ;
#18596 = CARTESIAN_POINT ( 'NONE',  ( 28.96193690644979668, 14.74639653023213093, 2.999999999999995559 ) ) ;
#18597 = CARTESIAN_POINT ( 'NONE',  ( 35.00000000000000711, 39.00000000000000711, -49.99999999999997868 ) ) ;
#18598 = CARTESIAN_POINT ( 'NONE',  ( -48.93401015228422324, 10.00000000000000000, -46.57614213197970088 ) ) ;
#18599 = VERTEX_POINT ( 'NONE', #19514 ) ;
#18600 = DIRECTION ( 'NONE',  ( -0.000000000000000000, -0.000000000000000000, -1.000000000000000000 ) ) ;
#18601 = DIRECTION ( 'NONE',  ( 6.505213034913038160E-19, 3.903127820947822896E-18, 1.000000000000000000 ) ) ;
#18602 = TOROIDAL_SURFACE ( 'NONE', #1405, 34.90673715956759082, 8.750000000000000000 ) ;
#18603 = EDGE_LOOP ( 'NONE', ( #13861, #16198, #5460, #7801 ) ) ;
#18604 = LINE ( 'NONE', #3019, #18160 ) ;
#18605 = CARTESIAN_POINT ( 'NONE',  ( -6.094386425459117795, 0.8904119427534493703, -54.73837739180613227 ) ) ;
#18606 = AXIS2_PLACEMENT_3D ( 'NONE', #10569, #7137, #21126 ) ;
#18607 = ORIENTED_EDGE ( 'NONE', *, *, #14768, .F. ) ;
#18608 = VECTOR ( 'NONE', #21404, 1000.000000000000000 ) ;
#18609 = AXIS2_PLACEMENT_3D ( 'NONE', #18388, #11293, #984 ) ;
#18610 = DIRECTION ( 'NONE',  ( -0.000000000000000000, -0.000000000000000000, -1.000000000000000000 ) ) ;
#18611 = FACE_OUTER_BOUND ( 'NONE', #653, .T. ) ;
#18612 = AXIS2_PLACEMENT_3D ( 'NONE', #12321, #19096, #8664 ) ;
#18613 = CARTESIAN_POINT ( 'NONE',  ( 18.97285531159653971, 26.38757670764486463, -60.36948798341702371 ) ) ;
#18615 = EDGE_CURVE ( 'NONE', #15608, #407, #17186, .T. ) ;
#18614 = ORIENTED_EDGE ( 'NONE', *, *, #17660, .F. ) ;
#18616 = ADVANCED_FACE ( 'NONE', ( #9087 ), #5316, .F. ) ;
#18617 = VERTEX_POINT ( 'NONE', #3608 ) ;
#18618 = AXIS2_PLACEMENT_3D ( 'NONE', #22674, #4789, #3408 ) ;
#18619 = ORIENTED_EDGE ( 'NONE', *, *, #19548, .F. ) ;
#18620 = AXIS2_PLACEMENT_3D ( 'NONE', #21314, #8937, #5504 ) ;
#18621 = ORIENTED_EDGE ( 'NONE', *, *, #16281, .T. ) ;
#18622 = CARTESIAN_POINT ( 'NONE',  ( 10.50000000000024514, -2.516660498395250745, 60.00099999999999767 ) ) ;
#18623 = VECTOR ( 'NONE', #17480, 1000.000000000000000 ) ;
#18624 = AXIS2_PLACEMENT_3D ( 'NONE', #14163, #18067, #8911 ) ;
#18625 = EDGE_CURVE ( 'NONE', #19349, #14184, #15715, .T. ) ;
#18626 = VERTEX_POINT ( 'NONE', #11365 ) ;
#18627 = DIRECTION ( 'NONE',  ( 1.296372316667914327E-16, 1.000000000000000000, -0.000000000000000000 ) ) ;
#18628 = CARTESIAN_POINT ( 'NONE',  ( -5.748506628232283866, -0.6819283742247831404, -52.01451867725678113 ) ) ;
#18629 = VERTEX_POINT ( 'NONE', #19966 ) ;
#18630 = VECTOR ( 'NONE', #5070, 1000.000000000000000 ) ;
#18631 = CARTESIAN_POINT ( 'NONE',  ( -1.572625745562107324, 13.32985487263445812, 6.879522542764194171 ) ) ;
#18632 = VERTEX_POINT ( 'NONE', #9538 ) ;
#18633 = CARTESIAN_POINT ( 'NONE',  ( 5.133463079812987218, 39.34078236626471892, -53.02544357726076640 ) ) ;
#18634 = CYLINDRICAL_SURFACE ( 'NONE', #5062, 19.11328065563152379 ) ;
#18635 = CARTESIAN_POINT ( 'NONE',  ( -35.52192638951989068, 1.010906942018126697, 3.000000000000041744 ) ) ;
#18636 = CARTESIAN_POINT ( 'NONE',  ( -13.65693838750921607, 34.64075751992690755, -58.69913499740199825 ) ) ;
#18637 = AXIS2_PLACEMENT_3D ( 'NONE', #14715, #12995, #21502 ) ;
#18638 = VECTOR ( 'NONE', #18468, 1000.000000000000000 ) ;
#18639 = ADVANCED_FACE ( 'NONE', ( #16291 ), #13177, .F. ) ;
#18640 = DIRECTION ( 'NONE',  ( -1.000000000000000000, 1.371829164384562918E-16, 0.000000000000000000 ) ) ;
#18641 = PRODUCT_DEFINITION_FORMATION_WITH_SPECIFIED_SOURCE ( 'ANY', '', #5829, .NOT_KNOWN. ) ;
#18642 = ORIENTED_EDGE ( 'NONE', *, *, #19229, .F. ) ;
#18643 = VERTEX_POINT ( 'NONE', #11249 ) ;
#18644 = ORIENTED_EDGE ( 'NONE', *, *, #15920, .T. ) ;
#18645 = CARTESIAN_POINT ( 'NONE',  ( -19.35294509712510092, 31.41613210955674518, 57.92571537617230604 ) ) ;
#18646 = DIRECTION ( 'NONE',  ( 6.505213034913038160E-19, 3.903127820947822896E-18, 1.000000000000000000 ) ) ;
#18647 = AXIS2_PLACEMENT_3D ( 'NONE', #16562, #18511, #11634 ) ;
#18648 = CARTESIAN_POINT ( 'NONE',  ( -15.59166974688846707, 7.467814210042477363, -59.37578565761233307 ) ) ;
#18649 = CYLINDRICAL_SURFACE ( 'NONE', #1226, 2.500000000000002220 ) ;
#18650 = ORIENTED_EDGE ( 'NONE', *, *, #10683, .T. ) ;
#18651 = CARTESIAN_POINT ( 'NONE',  ( 25.00000000000000000, 20.00000000000000000, 6.487780019669002523E-15 ) ) ;
#18652 = CARTESIAN_POINT ( 'NONE',  ( -1.387778780781445676E-14, 40.00000000000000000, -48.73397172404481381 ) ) ;
#18653 = CARTESIAN_POINT ( 'NONE',  ( 48.93401015228424455, 7.000000000000000000, -46.57614213197967956 ) ) ;
#18654 = DIRECTION ( 'NONE',  ( 0.000000000000000000, -1.000000000000000000, 0.000000000000000000 ) ) ;
#18655 = ADVANCED_FACE ( 'NONE', ( #4277 ), #9645, .F. ) ;
#18656 = PRODUCT_DEFINITION_SHAPE ( 'NONE', 'NONE',  #22699 ) ;
#18657 = PRODUCT_DEFINITION ( 'UNKNOWN', '', #17897, #2245 ) ;
#18658 = ORIENTED_EDGE ( 'NONE', *, *, #18472, .T. ) ;
#18659 = CARTESIAN_POINT ( 'NONE',  ( -35.00000000000000000, 15.00000000000000000, -40.99999999999997868 ) ) ;
#18660 = DIRECTION ( 'NONE',  ( 6.505213034913038160E-19, 3.903127820947822896E-18, 1.000000000000000000 ) ) ;
#18661 = EDGE_CURVE ( 'NONE', #8973, #11275, #19780, .T. ) ;
#18662 = ORIENTED_EDGE ( 'NONE', *, *, #21966, .T. ) ;
#18663 = CARTESIAN_POINT ( 'NONE',  ( -12.84899528830097104, 2.142135623730931471, -57.90797000640141334 ) ) ;
#18664 = CARTESIAN_POINT ( 'NONE',  ( -0.6841746959065087008, -36.75746821813308429, -2.800654218530457484 ) ) ;
#18665 = CARTESIAN_POINT ( 'NONE',  ( 35.00000000000000000, 13.99999999999999822, 2.255140518769849223E-14 ) ) ;
#18666 = ORIENTED_EDGE ( 'NONE', *, *, #12907, .T. ) ;
#18667 = ORIENTED_EDGE ( 'NONE', *, *, #3134, .F. ) ;
#18668 = CYLINDRICAL_SURFACE ( 'NONE', #21375, 19.11328065563151668 ) ;
#18669 = CIRCLE ( 'NONE', #8793, 19.11328065563152379 ) ;
#18670 = ADVANCED_FACE ( 'NONE', ( #16636 ), #5869, .T. ) ;
#18671 = FACE_OUTER_BOUND ( 'NONE', #186, .T. ) ;
#18672 = ORIENTED_EDGE ( 'NONE', *, *, #13343, .T. ) ;
#18673 = DIRECTION ( 'NONE',  ( 0.000000000000000000, 1.000000000000000000, 0.000000000000000000 ) ) ;
#18674 = AXIS2_PLACEMENT_3D ( 'NONE', #481, #14568, #17907 ) ;
#18675 = CARTESIAN_POINT ( 'NONE',  ( -2.347663744114047990, -31.41239365194231681, -2.999999999999995559 ) ) ;
#18676 = CARTESIAN_POINT ( 'NONE',  ( -47.83731665821552781, 6.999999999999999112, -38.93845529828707441 ) ) ;
#18677 = EDGE_CURVE ( 'NONE', #8182, #5375, #19857, .T. ) ;
#18678 = CARTESIAN_POINT ( 'NONE',  ( 13.85640646055130709, -25.00000000000000000, -4.000000000000099476 ) ) ;
#18679 = CARTESIAN_POINT ( 'NONE',  ( -14.05436202270911217, 25.29714423467776996, -45.40204559108963878 ) ) ;
#18680 = CARTESIAN_POINT ( 'NONE',  ( 90.00000000000000000, 26.00000000000000355, -9.108981535246192915E-16 ) ) ;
#18681 = VERTEX_POINT ( 'NONE', #6216 ) ;
#18682 = CARTESIAN_POINT ( 'NONE',  ( 42.49999999999998579, 7.000000000000000000, -53.99999999999997868 ) ) ;
#18683 = DIRECTION ( 'NONE',  ( -6.505213034913038160E-19, -3.903127820947822896E-18, -1.000000000000000000 ) ) ;
#18684 = CARTESIAN_POINT ( 'NONE',  ( 6.696867368503558448E-15, 0.000000000000000000, 38.73397172404480671 ) ) ;
#18685 = CARTESIAN_POINT ( 'NONE',  ( 35.00000000000000000, 0.000000000000000000, 4.258610482196280173E-15 ) ) ;
#18686 = VERTEX_POINT ( 'NONE', #21686 ) ;
#18687 = AXIS2_PLACEMENT_3D ( 'NONE', #3881, #15777, #3999 ) ;
#18688 = DIRECTION ( 'NONE',  ( -0.000000000000000000, -1.000000000000000000, -0.000000000000000000 ) ) ;
#18689 = FACE_OUTER_BOUND ( 'NONE', #22517, .T. ) ;
#18690 = ORIENTED_EDGE ( 'NONE', *, *, #4793, .T. ) ;
#18691 = EDGE_CURVE ( 'NONE', #7599, #1088, #6969, .T. ) ;
#18692 = ORIENTED_EDGE ( 'NONE', *, *, #16281, .F. ) ;
#18693 = CIRCLE ( 'NONE', #10623, 7.500000000000000000 ) ;
#18694 = ORIENTED_EDGE ( 'NONE', *, *, #12938, .F. ) ;
#18695 = DIRECTION ( 'NONE',  ( 0.000000000000000000, 0.000000000000000000, -1.000000000000000000 ) ) ;
#18696 = FACE_OUTER_BOUND ( 'NONE', #4782, .T. ) ;
#18697 = CIRCLE ( 'NONE', #21630, 2.499999999999995115 ) ;
#18698 = DIRECTION ( 'NONE',  ( 1.000000000000000000, 1.208970125616063490E-17, 0.000000000000000000 ) ) ;
#18699 = DIRECTION ( 'NONE',  ( -1.000000000000000000, 1.301042606982605814E-16, 0.000000000000000000 ) ) ;
#18700 = CARTESIAN_POINT ( 'NONE',  ( 8.646032897229204650, -31.21605069118105291, -2.999999999999981792 ) ) ;
#18701 = VERTEX_POINT ( 'NONE', #7705 ) ;
#18702 = LINE ( 'NONE', #6441, #10204 ) ;
#18703 = CARTESIAN_POINT ( 'NONE',  ( 34.64554704988886158, 10.35112103033863029, -2.932164912090505560 ) ) ;
#18704 = VERTEX_POINT ( 'NONE', #2670 ) ;
#18705 = ADVANCED_FACE ( 'NONE', ( #21805 ), #21608, .T. ) ;
#18706 = CARTESIAN_POINT ( 'NONE',  ( -12.70473862104220864, 11.99136930790644229, -44.75655646380167951 ) ) ;
#18707 = EDGE_CURVE ( 'NONE', #17173, #4023, #942, .T. ) ;
#18708 = CYLINDRICAL_SURFACE ( 'NONE', #22572, 4.000000000000000000 ) ;
#18709 = CARTESIAN_POINT ( 'NONE',  ( 4.080045426412798548, -32.20238537491815123, -2.999999999999971578 ) ) ;
#18710 = CARTESIAN_POINT ( 'NONE',  ( 8.776846306732625891, 39.47243301244805025, 54.19537464444116637 ) ) ;
#18711 = EDGE_LOOP ( 'NONE', ( #7797, #21734, #10794, #16158 ) ) ;
#18712 = CARTESIAN_POINT ( 'NONE',  ( -8.847970493949620874, 40.00000000000000711, -53.28481329731337723 ) ) ;
#18713 = ORIENTED_EDGE ( 'NONE', *, *, #3658, .F. ) ;
#18714 = CARTESIAN_POINT ( 'NONE',  ( 2.496587642955522490, 0.1153990516131240540, -52.32802461649443870 ) ) ;
#18715 = CARTESIAN_POINT ( 'NONE',  ( -0.4213896610233284767, -0.02267536297422790767, -49.14983462332308761 ) ) ;
#18716 = VERTEX_POINT ( 'NONE', #13065 ) ;
#18717 = FACE_OUTER_BOUND ( 'NONE', #22133, .T. ) ;
#18718 = CARTESIAN_POINT ( 'NONE',  ( 42.50000000000000711, -11.97499999999999964, -47.50000000000000000 ) ) ;
#18719 = EDGE_CURVE ( 'NONE', #18716, #6587, #10975, .T. ) ;
#18720 = DIRECTION ( 'NONE',  ( 0.000000000000000000, 0.000000000000000000, -1.000000000000000000 ) ) ;
#18721 = CARTESIAN_POINT ( 'NONE',  ( 15.40035801025553752, 32.79675990107260475, -56.74176776513677822 ) ) ;
#18722 = ORIENTED_EDGE ( 'NONE', *, *, #2636, .T. ) ;
#18723 = ORIENTED_EDGE ( 'NONE', *, *, #1155, .T. ) ;
#18724 = ORIENTED_EDGE ( 'NONE', *, *, #2466, .T. ) ;
#18725 = CYLINDRICAL_SURFACE ( 'NONE', #4725, 49.99999999999998579 ) ;
#18726 = ORIENTED_EDGE ( 'NONE', *, *, #13759, .T. ) ;
#18727 = CARTESIAN_POINT ( 'NONE',  ( 11.86180952233169705, 39.00000000000000000, 55.35904751184887118 ) ) ;
#18728 = CARTESIAN_POINT ( 'NONE',  ( 42.50000000000000711, -9.600000000000001421, -47.50000000000000000 ) ) ;
#18729 = VECTOR ( 'NONE', #3345, 1000.000000000000000 ) ;
#18730 = EDGE_LOOP ( 'NONE', ( #12081, #14721, #14364, #11105 ) ) ;
#18731 = DIRECTION ( 'NONE',  ( 6.505213034913038160E-19, 3.903127820947822896E-18, 1.000000000000000000 ) ) ;
#18732 = FACE_OUTER_BOUND ( 'NONE', #6603, .T. ) ;
#18733 = ORIENTED_EDGE ( 'NONE', *, *, #16157, .T. ) ;
#18734 = DIRECTION ( 'NONE',  ( 1.000000000000000000, 0.000000000000000000, 0.000000000000000000 ) ) ;
#18735 = VERTEX_POINT ( 'NONE', #21457 ) ;
#18736 = CARTESIAN_POINT ( 'NONE',  ( 8.331955809010628045, 38.18181818181817277, -56.36098470834072316 ) ) ;
#18737 = DIRECTION ( 'NONE',  ( 6.505213034913038160E-19, 3.903127820947822896E-18, 1.000000000000000000 ) ) ;
#18738 = DIRECTION ( 'NONE',  ( -1.000000000000000000, 0.000000000000000000, 0.000000000000000000 ) ) ;
#18739 = CARTESIAN_POINT ( 'NONE',  ( -16.16780438139469211, 31.78273399965604540, -59.56292242448184027 ) ) ;
#18740 = EDGE_CURVE ( 'NONE', #16794, #8525, #4781, .T. ) ;
#18741 = EDGE_CURVE ( 'NONE', #9197, #12493, #1110, .T. ) ;
#18742 = CONICAL_SURFACE ( 'NONE', #18374, 58.99999999999698730, 0.7853981633974447263 ) ;
#18743 = CARTESIAN_POINT ( 'NONE',  ( -12.06668108811419771, 11.08190912999966038, 44.43106897542665479 ) ) ;
#18744 = EDGE_CURVE ( 'NONE', #18953, #6097, #2319, .T. ) ;
#18745 = ORIENTED_EDGE ( 'NONE', *, *, #18280, .T. ) ;
#18746 = VERTEX_POINT ( 'NONE', #7814 ) ;
#18747 = ORIENTED_EDGE ( 'NONE', *, *, #20268, .T. ) ;
#18748 = CARTESIAN_POINT ( 'NONE',  ( -19.81218727895213405, 22.86772234701062700, 58.09777938301198219 ) ) ;
#18749 = DIRECTION ( 'NONE',  ( -1.000000000000000000, -1.208970125616081209E-17, 0.000000000000000000 ) ) ;
#18750 = B_SPLINE_CURVE_WITH_KNOTS ( 'NONE', 3,
 ( #19203, #7276, #5546, #278 ),
 .UNSPECIFIED., .F., .F.,
 ( 4, 4 ),
 ( 9.545285769565287186E-07, 0.001900595205834659795 ),
 .UNSPECIFIED. ) ;
#18751 = DIRECTION ( 'NONE',  ( 1.296372316667914327E-16, 1.000000000000000000, -0.000000000000000000 ) ) ;
#18752 = DIRECTION ( 'NONE',  ( 0.000000000000000000, 1.000000000000000000, 0.000000000000000000 ) ) ;
#18753 = CIRCLE ( 'NONE', #4859, 19.11328065563151668 ) ;
#18754 = AXIS2_PLACEMENT_3D ( 'NONE', #9343, #7284, #21486 ) ;
#18755 = DIRECTION ( 'NONE',  ( 6.505213034913038160E-19, 3.903127820947822896E-18, 1.000000000000000000 ) ) ;
#18756 = VERTEX_POINT ( 'NONE', #6101 ) ;
#18757 = CARTESIAN_POINT ( 'NONE',  ( -10.49999999999980282, -2.516660498395515866, -100.0000000000000000 ) ) ;
#18758 = CARTESIAN_POINT ( 'NONE',  ( -8.578904148414546071, 40.00000000000000711, -53.18551243551740981 ) ) ;
#18759 = CYLINDRICAL_SURFACE ( 'NONE', #21512, 2.500000000000002220 ) ;
#18760 = CARTESIAN_POINT ( 'NONE',  ( 11.86180952234068364, 38.99999999999457145, -55.35904751185260864 ) ) ;
#18761 = CIRCLE ( 'NONE', #18032, 2.500000000000002220 ) ;
#18762 = B_SPLINE_CURVE_WITH_KNOTS ( 'NONE', 3,
 ( #5169, #13726, #15448, #12143 ),
 .UNSPECIFIED., .F., .F.,
 ( 4, 4 ),
 ( 0.000000000000000000, 0.001590342073036645322 ),
 .UNSPECIFIED. ) ;
#18763 = ORIENTED_EDGE ( 'NONE', *, *, #10974, .F. ) ;
#18764 = CARTESIAN_POINT ( 'NONE',  ( -9.886810797454463895, 39.30595911725853142, 54.61697552269315992 ) ) ;
#18765 = ORIENTED_EDGE ( 'NONE', *, *, #19133, .F. ) ;
#18766 = DIRECTION ( 'NONE',  ( -6.505213034913038160E-19, -3.903127820947822896E-18, -1.000000000000000000 ) ) ;
#18767 = PLANE ( 'NONE',  #10405 ) ;
#18768 = CARTESIAN_POINT ( 'NONE',  ( 2.220446049250313081E-13, -2.498001805406602216E-13, -6.859353255829918616 ) ) ;
#18769 = FACE_BOUND ( 'NONE', #15746, .T. ) ;
#18770 = ORIENTED_EDGE ( 'NONE', *, *, #3565, .F. ) ;
#18771 = AXIS2_PLACEMENT_3D ( 'NONE', #21205, #19487, #3792 ) ;
#18772 = AXIS2_PLACEMENT_3D ( 'NONE', #8662, #14013, #5009 ) ;
#18773 = AXIS2_PLACEMENT_3D ( 'NONE', #8772, #15741, #53 ) ;
#18774 = ADVANCED_FACE ( 'NONE', ( #14896 ), #21923, .F. ) ;
#18775 = ORIENTED_EDGE ( 'NONE', *, *, #1179, .T. ) ;
#18776 = CARTESIAN_POINT ( 'NONE',  ( -8.466980083302928506, -4.900852744035391950, 50.56985808960192230 ) ) ;
#18777 = CARTESIAN_POINT ( 'NONE',  ( -7.711478842616386942, 31.57187188083510065, -2.999999999999971578 ) ) ;
#18778 = ORIENTED_EDGE ( 'NONE', *, *, #18490, .T. ) ;
#18779 = EDGE_CURVE ( 'NONE', #6315, #11727, #11131, .T. ) ;
#18780 = CARTESIAN_POINT ( 'NONE',  ( 14.50678847729821896, 16.16560534949676509, 45.60743157421821081 ) ) ;
#18781 = CARTESIAN_POINT ( 'NONE',  ( -2.855944605007508574, 34.72779906119552606, -39.14690304189947767 ) ) ;
#18782 = CARTESIAN_POINT ( 'NONE',  ( -42.50000000000000000, 7.000000000000000000, 47.49999999999999289 ) ) ;
#18783 = CARTESIAN_POINT ( 'NONE',  ( -19.97206123483410423, 21.14267036293994906, -58.14006880918119435 ) ) ;
#18784 = CARTESIAN_POINT ( 'NONE',  ( 2.220446049250313081E-13, -8.326672684688674053E-14, 2.800654218530498785 ) ) ;
#18785 = AXIS2_PLACEMENT_3D ( 'NONE', #8213, #10138, #13125 ) ;
#18786 = CARTESIAN_POINT ( 'NONE',  ( -15.62385314663568714, 32.51590977305111352, 59.38867318806723006 ) ) ;
#18787 = VERTEX_POINT ( 'NONE', #2444 ) ;
#18788 = DIRECTION ( 'NONE',  ( -6.505213034913038160E-19, -3.903127820947822896E-18, -1.000000000000000000 ) ) ;
#18789 = DIRECTION ( 'NONE',  ( 0.000000000000000000, 0.000000000000000000, 1.000000000000000000 ) ) ;
#18790 = CIRCLE ( 'NONE', #1234, 10.00000000000000000 ) ;
#18791 = CARTESIAN_POINT ( 'NONE',  ( -15.49999999999980460, -2.516660498395515866, 105.0000000000000142 ) ) ;
#18792 = DIRECTION ( 'NONE',  ( 0.000000000000000000, 1.000000000000000000, 0.000000000000000000 ) ) ;
#18793 = AXIS2_PLACEMENT_3D ( 'NONE', #12722, #468, #17658 ) ;
#18794 = ORIENTED_EDGE ( 'NONE', *, *, #7776, .T. ) ;
#18795 = DIRECTION ( 'NONE',  ( 6.505213034913038160E-19, 3.903127820947822896E-18, 1.000000000000000000 ) ) ;
#18796 = LINE ( 'NONE', #13609, #10908 ) ;
#18797 = CIRCLE ( 'NONE', #14008, 41.00000000000000000 ) ;
#18798 = ADVANCED_FACE ( 'NONE', ( #8267 ), #22483, .T. ) ;
#18799 = EDGE_LOOP ( 'NONE', ( #9133, #18520, #10504, #12568 ) ) ;
#18800 = AXIS2_PLACEMENT_3D ( 'NONE', #1769, #22635, #1652 ) ;
#18801 = ORIENTED_EDGE ( 'NONE', *, *, #22395, .T. ) ;
#18802 = VECTOR ( 'NONE', #13140, 1000.000000000000000 ) ;
#18803 = CONTEXT_DEPENDENT_SHAPE_REPRESENTATION ( #1260, #18656 ) ;
#18804 = CIRCLE ( 'NONE', #15861, 2.524999999999999467 ) ;
#18805 = ORIENTED_EDGE ( 'NONE', *, *, #16160, .F. ) ;
#18806 = DIRECTION ( 'NONE',  ( -1.000000000000000000, 0.000000000000000000, 0.000000000000000000 ) ) ;
#18807 = EDGE_CURVE ( 'NONE', #4282, #14096, #14355, .T. ) ;
#18808 = CARTESIAN_POINT ( 'NONE',  ( -3.000000000000000000, 15.20121272115292044, 8.485281374238567764 ) ) ;
#18809 = FACE_OUTER_BOUND ( 'NONE', #16058, .T. ) ;
#18810 = CARTESIAN_POINT ( 'NONE',  ( 14.06256854266893974, 5.693415384482566566, 58.85512087818932514 ) ) ;
#18811 = CARTESIAN_POINT ( 'NONE',  ( 35.00000000000001421, 0.000000000000000000, -58.99999999999701572 ) ) ;
#18812 = VERTEX_POINT ( 'NONE', #17192 ) ;
#18813 = CARTESIAN_POINT ( 'NONE',  ( 25.34312177887374062, -20.17230487860835453, -6.999999999999950262 ) ) ;
#18814 = CYLINDRICAL_SURFACE ( 'NONE', #18579, 19.11328065563151668 ) ;
#18815 = VERTEX_POINT ( 'NONE', #1391 ) ;
#18816 = DIRECTION ( 'NONE',  ( 0.000000000000000000, -1.000000000000000000, 0.000000000000000000 ) ) ;
#18817 = CARTESIAN_POINT ( 'NONE',  ( -2.836563456948004695E-15, -1.236374842841498678, -48.24164917503444627 ) ) ;
#18818 = DIRECTION ( 'NONE',  ( -0.000000000000000000, -0.000000000000000000, 1.000000000000000000 ) ) ;
#18819 = LINE ( 'NONE', #10092, #13035 ) ;
#18820 = ORIENTED_EDGE ( 'NONE', *, *, #7339, .T. ) ;
#18821 = DIRECTION ( 'NONE',  ( 0.000000000000000000, 0.000000000000000000, 1.000000000000000000 ) ) ;
#18822 = VERTEX_POINT ( 'NONE', #15236 ) ;
#18823 = DIRECTION ( 'NONE',  ( -1.000000000000000000, 0.000000000000000000, 0.000000000000000000 ) ) ;
#18824 = CONICAL_SURFACE ( 'NONE', #8928, 49.99999999999998579, 0.7853981633974657095 ) ;
#18825 = CARTESIAN_POINT ( 'NONE',  ( 5.074925817841801745, -32.10132595304126824, 3.000000000000023537 ) ) ;
#18826 = ORIENTED_EDGE ( 'NONE', *, *, #7908, .T. ) ;
#18827 = LINE ( 'NONE', #3363, #21505 ) ;
#18828 = ADVANCED_FACE ( 'NONE', ( #1506, #3233 ), #15460, .F. ) ;
#18829 = CARTESIAN_POINT ( 'NONE',  ( -34.99999999999999289, -5.000000000000000000, -54.99999999999705125 ) ) ;
#18830 = FACE_OUTER_BOUND ( 'NONE', #9754, .T. ) ;
#18831 = CARTESIAN_POINT ( 'NONE',  ( 22.38366207802858909, 18.39979965017225538, -58.65857802150448919 ) ) ;
#18832 = EDGE_CURVE ( 'NONE', #4080, #6950, #5038, .T. ) ;
#18833 = ADVANCED_FACE ( 'NONE', ( #20637 ), #22140, .F. ) ;
#18834 = VERTEX_POINT ( 'NONE', #20310 ) ;
#18835 = ORIENTED_EDGE ( 'NONE', *, *, #18415, .F. ) ;
#18836 = AXIS2_PLACEMENT_3D ( 'NONE', #15421, #13476, #18884 ) ;
#18837 = ORIENTED_EDGE ( 'NONE', *, *, #20630, .F. ) ;
#18838 = CARTESIAN_POINT ( 'NONE',  ( 35.00000000000000000, 40.00000000000000000, 4.258610482196280173E-15 ) ) ;
#18839 = EDGE_LOOP ( 'NONE', ( #1099, #40, #7021, #12530 ) ) ;
#18840 = CARTESIAN_POINT ( 'NONE',  ( -1.511556752833622896, 24.61754848632951465, 6.879730668860025489 ) ) ;
#18841 = CIRCLE ( 'NONE', #1651, 9.000000000000003553 ) ;
#18842 = DIRECTION ( 'NONE',  ( 0.000000000000000000, 0.000000000000000000, 1.000000000000000000 ) ) ;
#18843 = EDGE_CURVE ( 'NONE', #22196, #18519, #13077, .T. ) ;
#18844 = ORIENTED_EDGE ( 'NONE', *, *, #11357, .F. ) ;
#18845 = CARTESIAN_POINT ( 'NONE',  ( 5.551115123125782702E-14, -1.387778780781445676E-13, -5.749999999999949374 ) ) ;
#18846 = CARTESIAN_POINT ( 'NONE',  ( -4.026578693514479390, -4.679980696191891276, -48.24134193083673949 ) ) ;
#18847 = EDGE_LOOP ( 'NONE', ( #1076, #19052, #16870, #13650 ) ) ;
#18848 = CARTESIAN_POINT ( 'NONE',  ( 0.000000000000000000, 10.00000000000000000, 0.000000000000000000 ) ) ;
#18849 = EDGE_LOOP ( 'NONE', ( #13261, #1820, #21469, #14198 ) ) ;
#18850 = CARTESIAN_POINT ( 'NONE',  ( 9.786572406442770600, 39.51694226791492781, -54.52237350754640488 ) ) ;
#18851 = DIRECTION ( 'NONE',  ( -1.000000000000000000, 0.000000000000000000, 0.000000000000000000 ) ) ;
#18852 = VECTOR ( 'NONE', #7546, 1000.000000000000000 ) ;
#18853 = CARTESIAN_POINT ( 'NONE',  ( 6.696867368503558448E-15, 40.00000000000000000, 48.73397172404481381 ) ) ;
#18854 = CARTESIAN_POINT ( 'NONE',  ( -2.180214370012230507, 39.97139195390602140, 50.35379697857760561 ) ) ;
#18855 = EDGE_CURVE ( 'NONE', #16994, #21335, #22620, .T. ) ;
#18856 = AXIS2_PLACEMENT_3D ( 'NONE', #5358, #12335, #19345 ) ;
#18857 = CARTESIAN_POINT ( 'NONE',  ( -13.59841332577231299, 13.65742718326611715, 45.18857684126746221 ) ) ;
#18858 = ADVANCED_FACE ( 'NONE', ( #6555 ), #16966, .T. ) ;
#18859 = ORIENTED_EDGE ( 'NONE', *, *, #16424, .F. ) ;
#18860 = VERTEX_POINT ( 'NONE', #13517 ) ;
#18861 = ORIENTED_EDGE ( 'NONE', *, *, #12011, .F. ) ;
#18862 = AXIS2_PLACEMENT_3D ( 'NONE', #29, #21000, #5625 ) ;
#18863 = ADVANCED_FACE ( 'NONE', ( #20532 ), #8382, .F. ) ;
#18864 = VERTEX_POINT ( 'NONE', #16751 ) ;
#18865 = CARTESIAN_POINT ( 'NONE',  ( -11.86180952233172725, 39.00000000000000000, -55.35904751184885697 ) ) ;
#18866 = CARTESIAN_POINT ( 'NONE',  ( -24.73600648735095575, 27.19760187735845136, -2.800654218530457484 ) ) ;
#18867 = CONICAL_SURFACE ( 'NONE', #20331, 10.00000000000000000, 0.7853981633974447263 ) ;
#18868 = CARTESIAN_POINT ( 'NONE',  ( -16.97759837164273122, 9.398593820328095205, -59.81443117571819812 ) ) ;
#18869 = AXIS2_PLACEMENT_3D ( 'NONE', #8061, #19977, #7823 ) ;
#18870 = DIRECTION ( 'NONE',  ( 0.000000000000000000, -1.000000000000000000, 0.000000000000000000 ) ) ;
#18871 = AXIS2_PLACEMENT_3D ( 'NONE', #411, #10488, #19338 ) ;
#18872 = VERTEX_POINT ( 'NONE', #1058 ) ;
#18873 = CARTESIAN_POINT ( 'NONE',  ( -34.09180625983476176, -10.01331137436164020, -3.000000000000002220 ) ) ;
#18874 = CARTESIAN_POINT ( 'NONE',  ( 9.708269511265410046, -33.52953626616050542, -2.999999999999971578 ) ) ;
#18875 = DIRECTION ( 'NONE',  ( -1.000000000000000000, -1.208970125616063644E-17, 0.000000000000000000 ) ) ;
#18876 = CARTESIAN_POINT ( 'NONE',  ( 35.00000000000000000, 22.00000000000000711, 15.00000000000002132 ) ) ;
#18877 = EDGE_LOOP ( 'NONE', ( #4314, #346 ) ) ;
#18878 = DIRECTION ( 'NONE',  ( 6.505213034913038160E-19, 3.903127820947822896E-18, 1.000000000000000000 ) ) ;
#18879 = CONICAL_SURFACE ( 'NONE', #22189, 2.099999999999997868, 1.029744258676652091 ) ;
#18880 = AXIS2_PLACEMENT_3D ( 'NONE', #7267, #19526, #19424 ) ;
#18881 = ORIENTED_EDGE ( 'NONE', *, *, #9809, .T. ) ;
#18882 = DIRECTION ( 'NONE',  ( -1.000000000000000000, -8.894490888754757555E-15, 0.000000000000000000 ) ) ;
#18883 = CONICAL_SURFACE ( 'NONE', #11916, 58.99999999999994316, 0.7853981633974725929 ) ;
#18884 = DIRECTION ( 'NONE',  ( 0.000000000000000000, 0.000000000000000000, 1.000000000000000000 ) ) ;
#18885 = CARTESIAN_POINT ( 'NONE',  ( 19.99999999999998579, 20.00000000000000000, 60.62177826491070221 ) ) ;
#18886 = CARTESIAN_POINT ( 'NONE',  ( -5.010575289839672486, 34.16656919735249431, 40.02075074423078149 ) ) ;
#18887 = VERTEX_POINT ( 'NONE', #8050 ) ;
#18888 = AXIS2_PLACEMENT_3D ( 'NONE', #1699, #15660, #1352 ) ;
#18889 = EDGE_CURVE ( 'NONE', #4040, #14214, #5097, .T. ) ;
#18890 = EDGE_LOOP ( 'NONE', ( #4664, #17116, #4427, #19745, #15402, #133, #17567 ) ) ;
#18891 = CARTESIAN_POINT ( 'NONE',  ( -1.387778780781445676E-14, 20.00000000000000000, 60.00200000000000244 ) ) ;
#18892 = FACE_OUTER_BOUND ( 'NONE', #17129, .T. ) ;
#18893 = AXIS2_PLACEMENT_3D ( 'NONE', #9881, #10313, #8275 ) ;
#18894 = AXIS2_PLACEMENT_3D ( 'NONE', #9708, #21632, #778 ) ;
#18895 = CIRCLE ( 'NONE', #4644, 6.499999999999999112 ) ;
#18896 = ORIENTED_EDGE ( 'NONE', *, *, #21516, .F. ) ;
#18897 = VECTOR ( 'NONE', #9600, 1000.000000000000114 ) ;
#18898 = CARTESIAN_POINT ( 'NONE',  ( 14.94062893683334003, 18.45609313704556342, 45.79998742252196564 ) ) ;
#18899 = EDGE_CURVE ( 'NONE', #20510, #4801, #15121, .T. ) ;
#18900 = LINE ( 'NONE', #3207, #3028 ) ;
#18901 = CARTESIAN_POINT ( 'NONE',  ( 42.49999999999998579, 10.00000000000000000, -47.49999999999997868 ) ) ;
#18902 = CARTESIAN_POINT ( 'NONE',  ( -19.42731605661754202, 15.16896271047879807, -57.99434643146634727 ) ) ;
#18903 = CARTESIAN_POINT ( 'NONE',  ( -5.398822262509256120, 39.81726523789954086, 52.45277322177971513 ) ) ;
#18904 = CIRCLE ( 'NONE', #11949, 0.9999999999999974465 ) ;
#18905 = CARTESIAN_POINT ( 'NONE',  ( -13.87722263113804644, 34.42803545437053003, 58.77926695580350014 ) ) ;
#18906 = ORIENTED_EDGE ( 'NONE', *, *, #19425, .T. ) ;
#18907 = DIRECTION ( 'NONE',  ( -6.505213034913038160E-19, -3.903127820947822896E-18, -1.000000000000000000 ) ) ;
#18908 = FACE_BOUND ( 'NONE', #7549, .T. ) ;
#18909 = DIRECTION ( 'NONE',  ( 0.000000000000000000, -1.000000000000000000, 0.000000000000000000 ) ) ;
#18910 = CYLINDRICAL_SURFACE ( 'NONE', #15487, 2.499999999999995115 ) ;
#18911 = EDGE_CURVE ( 'NONE', #17759, #9582, #12151, .T. ) ;
#18912 = ORIENTED_EDGE ( 'NONE', *, *, #9895, .T. ) ;
#18913 = FACE_OUTER_BOUND ( 'NONE', #21811, .T. ) ;
#18914 = CARTESIAN_POINT ( 'NONE',  ( -32.40961249803532240, 2.422192751863672111, -2.999999999999960920 ) ) ;
#18915 = EDGE_CURVE ( 'NONE', #16909, #10389, #5069, .T. ) ;
#18916 = ORIENTED_EDGE ( 'NONE', *, *, #16230, .F. ) ;
#18917 = TOROIDAL_SURFACE ( 'NONE', #7196, 34.90673715956759082, 8.750000000000000000 ) ;
#18918 = SHAPE_DEFINITION_REPRESENTATION ( #21002, #8442 ) ;
#18919 = ORIENTED_EDGE ( 'NONE', *, *, #2266, .F. ) ;
#18920 = FACE_OUTER_BOUND ( 'NONE', #14056, .T. ) ;
#18921 = CARTESIAN_POINT ( 'NONE',  ( 3.309563215939714365, -3.140776953262784943, 49.61090469809098380 ) ) ;
#18922 = DIRECTION ( 'NONE',  ( -1.000000000000000000, 1.084202172485503941E-16, 0.000000000000000000 ) ) ;
#18923 = CARTESIAN_POINT ( 'NONE',  ( 19.99999999999998579, 20.00000000000000000, 60.62177826491070221 ) ) ;
#18924 = LINE ( 'NONE', #19041, #19363 ) ;
#18925 = VECTOR ( 'NONE', #19636, 1000.000000000000000 ) ;
#18926 = EDGE_LOOP ( 'NONE', ( #6599, #8170, #11509, #11169 ) ) ;
#18927 = DIRECTION ( 'NONE',  ( 0.000000000000000000, 0.000000000000000000, -1.000000000000000000 ) ) ;
#18928 = CARTESIAN_POINT ( 'NONE',  ( -25.58633464742622721, -23.74488952252778873, 3.000000000000002665 ) ) ;
#18929 = ORIENTED_EDGE ( 'NONE', *, *, #14097, .T. ) ;
#18930 = DIRECTION ( 'NONE',  ( 0.000000000000000000, 0.000000000000000000, 1.000000000000000000 ) ) ;
#18931 = VECTOR ( 'NONE', #20965, 1000.000000000000000 ) ;
#18932 = FACE_OUTER_BOUND ( 'NONE', #8831, .T. ) ;
#18933 = LINE ( 'NONE', #20542, #8623 ) ;
#18934 = ORIENTED_EDGE ( 'NONE', *, *, #9245, .F. ) ;
#18935 = CARTESIAN_POINT ( 'NONE',  ( 14.17374118098243940, 24.92453540474835805, -45.45638825402598826 ) ) ;
#18936 = ORIENTED_EDGE ( 'NONE', *, *, #12017, .F. ) ;
#18937 = CARTESIAN_POINT ( 'NONE',  ( 14.99999999999998579, 20.00000000000000000, -105.0020000000000095 ) ) ;
#18938 = DIRECTION ( 'NONE',  ( 6.505213034913038160E-19, 3.903127820947822896E-18, 1.000000000000000000 ) ) ;
#18939 = ADVANCED_FACE ( 'NONE', ( #5391 ), #11261, .T. ) ;
#18940 = ORIENTED_EDGE ( 'NONE', *, *, #3808, .T. ) ;
#18941 = DIRECTION ( 'NONE',  ( 6.505213034913038160E-19, 3.903127820947822896E-18, 1.000000000000000000 ) ) ;
#18942 = AXIS2_PLACEMENT_3D ( 'NONE', #12974, #7608, #5892 ) ;
#18943 = CIRCLE ( 'NONE', #10867, 41.00000000000000000 ) ;
#18944 = DIRECTION ( 'NONE',  ( 0.000000000000000000, 0.000000000000000000, -1.000000000000000000 ) ) ;
#18945 = DIRECTION ( 'NONE',  ( 0.000000000000000000, 0.000000000000000000, 1.000000000000000000 ) ) ;
#18946 = EDGE_CURVE ( 'NONE', #8364, #8988, #6866, .T. ) ;
#18947 = CIRCLE ( 'NONE', #4316, 59.99999999999700862 ) ;
#18948 = CARTESIAN_POINT ( 'NONE',  ( 12.37316313323383632, 4.263667856435456649, -58.19925355777955644 ) ) ;
#18949 = CIRCLE ( 'NONE', #16379, 34.90673715956759082 ) ;
#18950 = AXIS2_PLACEMENT_3D ( 'NONE', #21862, #6162, #4445 ) ;
#18951 = ORIENTED_EDGE ( 'NONE', *, *, #7775, .T. ) ;
#18952 = ORIENTED_EDGE ( 'NONE', *, *, #7404, .F. ) ;
#18953 = VERTEX_POINT ( 'NONE', #9055 ) ;
#18954 = PLANE ( 'NONE',  #14936 ) ;
#18955 = EDGE_LOOP ( 'NONE', ( #22420, #11993, #1780, #20497 ) ) ;
#18956 = CARTESIAN_POINT ( 'NONE',  ( -11.93972437435537870, -29.14949368109895289, -6.999999999999992006 ) ) ;
#18957 = CARTESIAN_POINT ( 'NONE',  ( 21.90353326617355023, 15.16496266307568774, 58.55331524747137451 ) ) ;
#18958 = CARTESIAN_POINT ( 'NONE',  ( -35.00000000000058265, 39.97500000000000142, -55.00000000000076028 ) ) ;
#18959 = EDGE_CURVE ( 'NONE', #7430, #15875, #18184, .T. ) ;
#18960 = SHAPE_REPRESENTATION ( 'GEAR', ( #18273 ), #12407 ) ;
#18961 = VERTEX_POINT ( 'NONE', #13858 ) ;
#18962 = FACE_BOUND ( 'NONE', #16604, .T. ) ;
#18963 = DIRECTION ( 'NONE',  ( 6.505213034913038160E-19, 3.903127820947822896E-18, 1.000000000000000000 ) ) ;
#18964 = ORIENTED_EDGE ( 'NONE', *, *, #5165, .F. ) ;
#18965 = CIRCLE ( 'NONE', #16376, 19.11328065563152023 ) ;
#18966 = CYLINDRICAL_SURFACE ( 'NONE', #9462, 2.500000000000002220 ) ;
#18967 = ORIENTED_EDGE ( 'NONE', *, *, #19838, .T. ) ;
#18968 = DIRECTION ( 'NONE',  ( -6.505213034913038160E-19, -3.903127820947822896E-18, -1.000000000000000000 ) ) ;
#18969 = CIRCLE ( 'NONE', #2131, 57.07106781186551103 ) ;
#18970 = DIRECTION ( 'NONE',  ( 1.000000000000000000, 1.208970125616063028E-17, 0.000000000000000000 ) ) ;
#18971 = ADVANCED_FACE ( 'NONE', ( #20873 ), #16371, .T. ) ;
#18972 = CARTESIAN_POINT ( 'NONE',  ( -2.931973760223107522E-15, -2.515546993500582751, -47.48752710978099145 ) ) ;
#18973 = CIRCLE ( 'NONE', #16400, 1.000000000000000888 ) ;
#18974 = CARTESIAN_POINT ( 'NONE',  ( -3.072149649144736649, 39.94358005063767791, 50.97360058146784212 ) ) ;
#18975 = DIRECTION ( 'NONE',  ( -1.000000000000000000, 0.000000000000000000, 0.000000000000000000 ) ) ;
#18976 = LINE ( 'NONE', #3507, #15653 ) ;
#18977 = APPLICATION_CONTEXT ( 'automotive_design' ) ;
#18978 = CARTESIAN_POINT ( 'NONE',  ( -14.87996495114181350, 18.06670563205965152, 45.77322900830828445 ) ) ;
#18979 = CIRCLE ( 'NONE', #13816, 2.500000000000002220 ) ;
#18980 = ORIENTED_EDGE ( 'NONE', *, *, #15566, .T. ) ;
#18981 = CIRCLE ( 'NONE', #9460, 17.00000000000000000 ) ;
#18982 = VECTOR ( 'NONE', #16300, 1000.000000000000000 ) ;
#18983 = EDGE_LOOP ( 'NONE', ( #6285, #10936, #21591, #4466, #22090, #20843, #4241, #14179, #16545 ) ) ;
#18984 = VERTEX_POINT ( 'NONE', #5177 ) ;
#18985 = AXIS2_PLACEMENT_3D ( 'NONE', #12152, #17193, #17641 ) ;
#18986 = ORIENTED_EDGE ( 'NONE', *, *, #12408, .F. ) ;
#18987 = DIRECTION ( 'NONE',  ( -1.000000000000000000, -1.208970125616063644E-17, 0.000000000000000000 ) ) ;
#18988 = CARTESIAN_POINT ( 'NONE',  ( 5.551115123125782702E-14, -1.387778780781445676E-13, -5.749999999999949374 ) ) ;
#18989 = EDGE_CURVE ( 'NONE', #6106, #18225, #20051, .T. ) ;
#18990 = DIRECTION ( 'NONE',  ( -0.000000000000000000, -1.000000000000000000, -0.000000000000000000 ) ) ;
#18991 = CARTESIAN_POINT ( 'NONE',  ( -9.952189117650803496, 40.00000000000000000, 53.64426396172073908 ) ) ;
#18992 = VECTOR ( 'NONE', #20704, 1000.000000000000000 ) ;
#18993 = VERTEX_POINT ( 'NONE', #1734 ) ;
#18994 = CARTESIAN_POINT ( 'NONE',  ( -42.50000000000000000, 10.00000000000000000, 49.99999999999999289 ) ) ;
#18995 = CARTESIAN_POINT ( 'NONE',  ( -7.563456402248210253, 40.00000000000000711, -52.78701496912255919 ) ) ;
#18996 = ADVANCED_FACE ( 'NONE', ( #13958 ), #17835, .T. ) ;
#18997 = LINE ( 'NONE', #13350, #9057 ) ;
#18998 = EDGE_CURVE ( 'NONE', #17558, #10689, #20979, .T. ) ;
#18999 = CARTESIAN_POINT ( 'NONE',  ( 42.50000000000000711, -12.00000000000000000, 47.50000000000000711 ) ) ;
#19000 = FILL_AREA_STYLE ('',( #21048 ) ) ;
#19001 = EDGE_LOOP ( 'NONE', ( #11109, #15818, #20730, #21407 ) ) ;
#19002 = CARTESIAN_POINT ( 'NONE',  ( -8.331955809010628045, 38.18181818181818699, 56.36098470834075158 ) ) ;
#19003 = AXIS2_PLACEMENT_3D ( 'NONE', #6096, #21916, #18242 ) ;
#19004 = ORIENTED_EDGE ( 'NONE', *, *, #3594, .T. ) ;
#19005 = CARTESIAN_POINT ( 'NONE',  ( -16.06969024216335740, -19.15111107797456924, -2.999999999999995559 ) ) ;
#19006 = DIRECTION ( 'NONE',  ( -1.000000000000000000, 0.000000000000000000, 0.000000000000000000 ) ) ;
#19007 = FACE_OUTER_BOUND ( 'NONE', #19839, .T. ) ;
#19008 = EDGE_CURVE ( 'NONE', #7125, #20382, #10154, .T. ) ;
#19009 = VERTEX_POINT ( 'NONE', #12472 ) ;
#19010 =( GEOMETRIC_REPRESENTATION_CONTEXT ( 3 ) GLOBAL_UNCERTAINTY_ASSIGNED_CONTEXT ( ( #2553 ) ) GLOBAL_UNIT_ASSIGNED_CONTEXT ( ( #19676, #4202, #10952 ) ) REPRESENTATION_CONTEXT ( 'NONE', 'WORKASPACE' ) );
#19011 = VERTEX_POINT ( 'NONE', #7722 ) ;
#19012 = CARTESIAN_POINT ( 'NONE',  ( 2.220446049250313081E-13, -2.498001805406602216E-13, -6.859353255829918616 ) ) ;
#19013 = CARTESIAN_POINT ( 'NONE',  ( 23.65408649739131164, 22.22891329980528141, -6.999999999999950262 ) ) ;
#19014 = ORIENTED_EDGE ( 'NONE', *, *, #20881, .F. ) ;
#19015 = CARTESIAN_POINT ( 'NONE',  ( 14.05436202270908375, 14.70285576532224425, 45.40204559108965299 ) ) ;
#19016 = DIRECTION ( 'NONE',  ( 0.000000000000000000, 0.000000000000000000, -1.000000000000000000 ) ) ;
#19017 = LINE ( 'NONE', #15327, #19329 ) ;
#19018 = CARTESIAN_POINT ( 'NONE',  ( -19.96591191797318388, 18.54839033250632241, -58.13845218885094823 ) ) ;
#19019 = CARTESIAN_POINT ( 'NONE',  ( 35.00000000000001421, 1.000000000000044187, 1.540743955509788682E-30 ) ) ;
#19020 = AXIS2_PLACEMENT_3D ( 'NONE', #19763, #18023, #4069 ) ;
#19021 = ORIENTED_EDGE ( 'NONE', *, *, #18575, .T. ) ;
#19022 = CYLINDRICAL_SURFACE ( 'NONE', #13425, 2.499999999999998668 ) ;
#19023 = FACE_OUTER_BOUND ( 'NONE', #19062, .T. ) ;
#19024 = DIRECTION ( 'NONE',  ( 0.000000000000000000, 0.000000000000000000, 1.000000000000000000 ) ) ;
#19025 = CARTESIAN_POINT ( 'NONE',  ( 7.463862311151453710, 35.99819890246955367, 2.800654218530485018 ) ) ;
#19026 = EDGE_CURVE ( 'NONE', #5986, #6323, #13300, .T. ) ;
#19027 = ORIENTED_EDGE ( 'NONE', *, *, #20572, .T. ) ;
#19028 = ADVANCED_FACE ( 'NONE', ( #9330 ), #6133, .T. ) ;
#19029 = DIRECTION ( 'NONE',  ( 6.505213034913038160E-19, 3.903127820947822896E-18, 1.000000000000000000 ) ) ;
#19030 = DIRECTION ( 'NONE',  ( -6.505213034913038160E-19, -3.903127820947822896E-18, -1.000000000000000000 ) ) ;
#19031 = CARTESIAN_POINT ( 'NONE',  ( 35.00000000000001421, 0.000000000000000000, 1.540743955509788682E-30 ) ) ;
#19032 = CIRCLE ( 'NONE', #16469, 15.00000000000000000 ) ;
#19033 = EDGE_CURVE ( 'NONE', #8887, #13337, #7954, .T. ) ;
#19034 = ORIENTED_EDGE ( 'NONE', *, *, #8808, .T. ) ;
#19035 = VECTOR ( 'NONE', #5805, 1000.000000000000000 ) ;
#19036 = PRODUCT_CONTEXT ( 'NONE', #15427, 'mechanical' ) ;
#19037 = ORIENTED_EDGE ( 'NONE', *, *, #13890, .F. ) ;
#19038 = CARTESIAN_POINT ( 'NONE',  ( 6.696867368503558448E-15, 39.00000000000000711, 38.73397172404480671 ) ) ;
#19039 = CARTESIAN_POINT ( 'NONE',  ( 5.079212789370819436, -3.097595057461635992, 50.74825967503632285 ) ) ;
#19040 = CARTESIAN_POINT ( 'NONE',  ( 14.29266125237896290, -28.07080038625095497, -2.999999999999971578 ) ) ;
#19041 = CARTESIAN_POINT ( 'NONE',  ( 35.00000000000000000, 25.00000000000000000, 9.000000000000007105 ) ) ;
#19042 = EDGE_LOOP ( 'NONE', ( #13552, #7648 ) ) ;
#19043 = CARTESIAN_POINT ( 'NONE',  ( 42.50000000000000711, -5.000000000000000000, 47.50000000000000711 ) ) ;
#19044 = DIRECTION ( 'NONE',  ( 6.505213034913038160E-19, 3.903127820947822896E-18, 1.000000000000000000 ) ) ;
#19045 = ORIENTED_EDGE ( 'NONE', *, *, #4379, .F. ) ;
#19046 = DIRECTION ( 'NONE',  ( 0.000000000000000000, 0.000000000000000000, 1.000000000000000000 ) ) ;
#19047 = DIRECTION ( 'NONE',  ( 6.505213034913038160E-19, 3.903127820947822896E-18, 1.000000000000000000 ) ) ;
#19049 = VECTOR ( 'NONE', #16670, 1000.000000000000000 ) ;
#19048 = CARTESIAN_POINT ( 'NONE',  ( -9.576564013118654017, 26.31139338200516420, -2.999999999999978240 ) ) ;
#19050 = DIRECTION ( 'NONE',  ( -6.505213034913038160E-19, -3.903127820947822896E-18, -1.000000000000000000 ) ) ;
#19051 = CARTESIAN_POINT ( 'NONE',  ( 11.13407802442741179, 30.05807871779232343, -43.93745127716449872 ) ) ;
#19052 = ORIENTED_EDGE ( 'NONE', *, *, #11440, .F. ) ;
#19053 = DIRECTION ( 'NONE',  ( 0.000000000000000000, -1.000000000000000000, 0.000000000000000000 ) ) ;
#19054 = CARTESIAN_POINT ( 'NONE',  ( -42.50000000000000711, -12.00000000000000000, 50.00000000000000711 ) ) ;
#19055 = ORIENTED_EDGE ( 'NONE', *, *, #15054, .F. ) ;
#19056 = CARTESIAN_POINT ( 'NONE',  ( -6.742883674876437361, -34.24928931925796860, 3.000000000000002665 ) ) ;
#19057 = CARTESIAN_POINT ( 'NONE',  ( 35.00000000000000000, 14.00000000000000000, 2.365113165210053967E-14 ) ) ;
#19058 = CYLINDRICAL_SURFACE ( 'NONE', #10352, 19.99999999999999289 ) ;
#19059 = CARTESIAN_POINT ( 'NONE',  ( 15.23870778339282772, 7.010517948053573534, -56.68442755504732133 ) ) ;
#19060 = ORIENTED_EDGE ( 'NONE', *, *, #13408, .F. ) ;
#19061 = CIRCLE ( 'NONE', #20530, 18.00000000000000355 ) ;
#19062 = EDGE_LOOP ( 'NONE', ( #22388, #8876 ) ) ;
#19063 = ORIENTED_EDGE ( 'NONE', *, *, #16424, .T. ) ;
#19064 = DIRECTION ( 'NONE',  ( 0.000000000000000000, 0.000000000000000000, -1.000000000000000000 ) ) ;
#19065 = EDGE_CURVE ( 'NONE', #17245, #1538, #20412, .T. ) ;
#19066 = ORIENTED_EDGE ( 'NONE', *, *, #21587, .T. ) ;
#19067 = DIRECTION ( 'NONE',  ( 8.659560562354903276E-17, -0.7071067811865500152, 0.7071067811865451302 ) ) ;
#19068 = CARTESIAN_POINT ( 'NONE',  ( 35.00000000000000711, 40.00000000000000000, 49.99999999999999289 ) ) ;
#19069 = DIRECTION ( 'NONE',  ( 0.000000000000000000, 0.000000000000000000, -1.000000000000000000 ) ) ;
#19070 = ADVANCED_FACE ( 'NONE', ( #21704 ), #16308, .T. ) ;
#19071 = ORIENTED_EDGE ( 'NONE', *, *, #11796, .T. ) ;
#19072 = CYLINDRICAL_SURFACE ( 'NONE', #11281, 2.500000000000002220 ) ;
#19073 = DIRECTION ( 'NONE',  ( -0.000000000000000000, -0.000000000000000000, 1.000000000000000000 ) ) ;
#19074 = EDGE_LOOP ( 'NONE', ( #19402, #22693 ) ) ;
#19075 = EDGE_CURVE ( 'NONE', #3715, #66, #12861, .T. ) ;
#19076 = EDGE_CURVE ( 'NONE', #7279, #10462, #6574, .T. ) ;
#19077 = CARTESIAN_POINT ( 'NONE',  ( -3.591923118226331086E-15, -5.000000000000000000, -44.98888751680799203 ) ) ;
#19078 = ORIENTED_EDGE ( 'NONE', *, *, #22598, .T. ) ;
#19079 = CARTESIAN_POINT ( 'NONE',  ( 6.450245752248383369, 39.75603576625821489, -53.02615179544272905 ) ) ;
#19080 = CARTESIAN_POINT ( 'NONE',  ( -8.485281374238567764, -3.000000000000002665, -6.859353255829953255 ) ) ;
#19081 = LINE ( 'NONE', #10347, #8769 ) ;
#19082 = CARTESIAN_POINT ( 'NONE',  ( 34.13396246814587442, -14.93538271375421900, 3.000000000000023537 ) ) ;
#19083 = LINE ( 'NONE', #8872, #10331 ) ;
#19084 = CARTESIAN_POINT ( 'NONE',  ( -10.00000000000000000, 1.499999999999997780, 3.000000000000000000 ) ) ;
#19085 = ADVANCED_FACE ( 'NONE', ( #6458 ), #10217, .T. ) ;
#19086 = ORIENTED_EDGE ( 'NONE', *, *, #2868, .T. ) ;
#19087 = AXIS2_PLACEMENT_3D ( 'NONE', #17785, #14329, #5635 ) ;
#19088 = AXIS2_PLACEMENT_3D ( 'NONE', #13278, #11477, #9760 ) ;
#19089 = ORIENTED_EDGE ( 'NONE', *, *, #18319, .F. ) ;
#19090 = ORIENTED_EDGE ( 'NONE', *, *, #2072, .T. ) ;
#19091 = EDGE_CURVE ( 'NONE', #15368, #8029, #4563, .T. ) ;
#19092 = ORIENTED_EDGE ( 'NONE', *, *, #6352, .F. ) ;
#19093 = DIRECTION ( 'NONE',  ( -1.000000000000000000, -0.000000000000000000, -0.000000000000000000 ) ) ;
#19094 = CARTESIAN_POINT ( 'NONE',  ( 35.00000000000001421, 1.000000000000044187, 1.540743955509788682E-30 ) ) ;
#19095 = DIRECTION ( 'NONE',  ( -1.000000000000000000, 1.371829164384562918E-16, 0.000000000000000000 ) ) ;
#19096 = DIRECTION ( 'NONE',  ( 6.505213034913038160E-19, 3.903127820947822896E-18, 1.000000000000000000 ) ) ;
#19097 = CARTESIAN_POINT ( 'NONE',  ( 1.619910636035357454, 39.98468599264958101, 49.95346646087499920 ) ) ;
#19098 = ADVANCED_FACE ( 'NONE', ( #20773 ), #5192, .T. ) ;
#19099 = EDGE_LOOP ( 'NONE', ( #14875, #7105, #5968, #5888 ) ) ;
#19100 = DIRECTION ( 'NONE',  ( -0.000000000000000000, -1.000000000000000000, -0.000000000000000000 ) ) ;
#19101 = DIRECTION ( 'NONE',  ( 0.000000000000000000, 1.000000000000000000, 0.000000000000000000 ) ) ;
#19102 = FACE_OUTER_BOUND ( 'NONE', #16791, .T. ) ;
#19103 = CARTESIAN_POINT ( 'NONE',  ( 1.110223024625156540E-13, -27.99999999999996803, -4.999999999999948486 ) ) ;
#19104 = LINE ( 'NONE', #20941, #1059 ) ;
#19105 = CIRCLE ( 'NONE', #814, 50.00000000000001421 ) ;
#19106 = EDGE_LOOP ( 'NONE', ( #4729, #15003 ) ) ;
#19107 = FACE_OUTER_BOUND ( 'NONE', #13995, .T. ) ;
#19108 = DIRECTION ( 'NONE',  ( -6.505213034913038160E-19, -3.903127820947822896E-18, -1.000000000000000000 ) ) ;
#19109 = ORIENTED_EDGE ( 'NONE', *, *, #9213, .T. ) ;
#19110 = DIRECTION ( 'NONE',  ( 6.505213034913038160E-19, 3.903127820947822896E-18, 1.000000000000000000 ) ) ;
#19111 = CARTESIAN_POINT ( 'NONE',  ( -8.234904025113911175, 38.24530784312006659, 54.56725976436211312 ) ) ;
#19112 = EDGE_CURVE ( 'NONE', #7355, #3909, #1006, .T. ) ;
#19113 = FACE_OUTER_BOUND ( 'NONE', #2805, .T. ) ;
#19114 = CARTESIAN_POINT ( 'NONE',  ( 28.95348479018588961, -14.76298474240531000, -2.999999999999999112 ) ) ;
#19115 = ORIENTED_EDGE ( 'NONE', *, *, #22505, .T. ) ;
#19116 = VERTEX_POINT ( 'NONE', #13637 ) ;
#19117 = EDGE_CURVE ( 'NONE', #4006, #21260, #22247, .T. ) ;
#19118 = ORIENTED_EDGE ( 'NONE', *, *, #9384, .F. ) ;
#19119 = CARTESIAN_POINT ( 'NONE',  ( 3.174475770762294591, -4.645331003335221531, -47.72510079650860604 ) ) ;
#19120 = AXIS2_PLACEMENT_3D ( 'NONE', #2351, #19437, #2124 ) ;
#19121 = CARTESIAN_POINT ( 'NONE',  ( 10.75185716664280555, 39.99999999999999289, -53.88525272612032069 ) ) ;
#19122 = ORIENTED_EDGE ( 'NONE', *, *, #4999, .T. ) ;
#19123 = DIRECTION ( 'NONE',  ( 6.505213034913038160E-19, 3.903127820947822896E-18, 1.000000000000000000 ) ) ;
#19124 = ADVANCED_FACE ( 'NONE', ( #13758 ), #20443, .T. ) ;
#19125 = LINE ( 'NONE', #13594, #12882 ) ;
#19126 = FACE_OUTER_BOUND ( 'NONE', #15388, .T. ) ;
#19127 = CARTESIAN_POINT ( 'NONE',  ( -18.02527238916006525, 28.84533800490841671, -60.11925852859477004 ) ) ;
#19128 = LINE ( 'NONE', #6985, #21059 ) ;
#19129 = ORIENTED_EDGE ( 'NONE', *, *, #19091, .T. ) ;
#19130 = DIRECTION ( 'NONE',  ( 1.000000000000000000, 0.000000000000000000, 0.000000000000000000 ) ) ;
#19131 = DIRECTION ( 'NONE',  ( -0.000000000000000000, 1.000000000000000000, -0.000000000000000000 ) ) ;
#19132 = DIRECTION ( 'NONE',  ( -0.000000000000000000, -0.000000000000000000, 1.000000000000000000 ) ) ;
#19133 = EDGE_CURVE ( 'NONE', #20269, #7645, #5087, .T. ) ;
#19134 = DIRECTION ( 'NONE',  ( -0.000000000000000000, -0.000000000000000000, 1.000000000000000000 ) ) ;
#19135 = CARTESIAN_POINT ( 'NONE',  ( -34.99999999999980815, 40.00000000000000000, 52.49999999999922551 ) ) ;
#19136 = AXIS2_PLACEMENT_3D ( 'NONE', #16722, #6297, #8133 ) ;
#19137 = ORIENTED_EDGE ( 'NONE', *, *, #9026, .T. ) ;
#19138 = AXIS2_PLACEMENT_3D ( 'NONE', #13652, #1534, #20788 ) ;
#19139 = EDGE_CURVE ( 'NONE', #1737, #260, #3591, .T. ) ;
#19140 = LINE ( 'NONE', #5492, #3521 ) ;
#19141 = DIRECTION ( 'NONE',  ( -6.505213034913038160E-19, -3.903127820947822896E-18, -1.000000000000000000 ) ) ;
#19142 = VECTOR ( 'NONE', #17583, 1000.000000000000000 ) ;
#19143 = ORIENTED_EDGE ( 'NONE', *, *, #20577, .T. ) ;
#19144 = PRODUCT_CONTEXT ( 'NONE', #1399, 'mechanical' ) ;
#19145 = ADVANCED_FACE ( 'NONE', ( #17317 ), #9892, .F. ) ;
#19146 = VERTEX_POINT ( 'NONE', #11721 ) ;
#19147 = CYLINDRICAL_SURFACE ( 'NONE', #1895, 22.12933039895921539 ) ;
#19148 = CARTESIAN_POINT ( 'NONE',  ( 3.001573872049483782, -1.099462678413573036, 50.31569927527682040 ) ) ;
#19149 = CARTESIAN_POINT ( 'NONE',  ( -7.474202570535936729, 30.60042966911702322, -7.000000000000006217 ) ) ;
#19150 = ADVANCED_FACE ( 'NONE', ( #18717 ), #22499, .F. ) ;
#19151 = CIRCLE ( 'NONE', #12194, 14.00000000000000000 ) ;
#19152 = DIRECTION ( 'NONE',  ( 0.000000000000000000, 0.000000000000000000, 1.000000000000000000 ) ) ;
#19153 = CARTESIAN_POINT ( 'NONE',  ( -42.50000000000000711, -12.00000000000000000, 41.00000000000000711 ) ) ;
#19154 = VERTEX_POINT ( 'NONE', #19056 ) ;
#19155 = DIRECTION ( 'NONE',  ( -1.000000000000000000, 0.000000000000000000, 0.000000000000000000 ) ) ;
#19156 = AXIS2_PLACEMENT_3D ( 'NONE', #5890, #11149, #12859 ) ;
#19157 = ORIENTED_EDGE ( 'NONE', *, *, #775, .F. ) ;
#19158 = DIRECTION ( 'NONE',  ( -0.000000000000000000, 1.000000000000000000, -0.000000000000000000 ) ) ;
#19159 = VECTOR ( 'NONE', #1181, 1000.000000000000000 ) ;
#19160 = CYLINDRICAL_SURFACE ( 'NONE', #16699, 10.00000000000000178 ) ;
#19161 = DIRECTION ( 'NONE',  ( 6.505213034913038160E-19, 3.903127820947822896E-18, 1.000000000000000000 ) ) ;
#19162 = DIRECTION ( 'NONE',  ( -0.000000000000000000, -1.000000000000000000, -0.000000000000000000 ) ) ;
#19163 = CARTESIAN_POINT ( 'NONE',  ( -9.455104433789056628, 39.37252125230245525, -54.46735621690890383 ) ) ;
#19164 = EDGE_CURVE ( 'NONE', #7946, #8065, #18827, .T. ) ;
#19165 = ORIENTED_EDGE ( 'NONE', *, *, #8006, .T. ) ;
#19166 = CARTESIAN_POINT ( 'NONE',  ( -21.00948735876881202, -24.79619811426206510, -2.999999999999995559 ) ) ;
#19167 = LINE ( 'NONE', #3474, #4574 ) ;
#19168 = EDGE_LOOP ( 'NONE', ( #5426, #13706 ) ) ;
#19169 = DIRECTION ( 'NONE',  ( -0.000000000000000000, -1.000000000000000000, -0.000000000000000000 ) ) ;
#19170 = DIRECTION ( 'NONE',  ( -6.505213034913038160E-19, -3.903127820947822896E-18, -1.000000000000000000 ) ) ;
#19171 = CARTESIAN_POINT ( 'NONE',  ( 35.00000000000000000, 2.142135623730931471, 4.258610482196280173E-15 ) ) ;
#19172 = CIRCLE ( 'NONE', #20612, 2.500000000000002220 ) ;
#19173 = AXIS2_PLACEMENT_3D ( 'NONE', #15898, #5713, #7202 ) ;
#19174 = CIRCLE ( 'NONE', #13275, 20.00000000000002132 ) ;
#19175 = VERTEX_POINT ( 'NONE', #9990 ) ;
#19176 = ORIENTED_EDGE ( 'NONE', *, *, #11948, .T. ) ;
#19177 = EDGE_LOOP ( 'NONE', ( #7715, #15316, #7921, #13319 ) ) ;
#19178 = CARTESIAN_POINT ( 'NONE',  ( -10.00000000000000000, -4.824555320336763486, 3.000000000000000000 ) ) ;
#19179 = EDGE_CURVE ( 'NONE', #9796, #21104, #15271, .T. ) ;
#19180 = ORIENTED_EDGE ( 'NONE', *, *, #15433, .T. ) ;
#19181 = CARTESIAN_POINT ( 'NONE',  ( -35.00000000000000000, 14.00000000000000000, 39.00000000000002132 ) ) ;
#19182 = CARTESIAN_POINT ( 'NONE',  ( 22.30616949375635727, 22.91984106672850174, 58.64191913087365293 ) ) ;
#19183 = AXIS2_PLACEMENT_3D ( 'NONE', #12440, #17718, #19454 ) ;
#19184 = DIRECTION ( 'NONE',  ( -0.000000000000000000, -1.000000000000000000, -0.000000000000000000 ) ) ;
#19185 = CARTESIAN_POINT ( 'NONE',  ( 8.616492322300894457, 39.99999999999999289, 53.19943576118269135 ) ) ;
#19186 = ORIENTED_EDGE ( 'NONE', *, *, #21793, .F. ) ;
#19187 = CARTESIAN_POINT ( 'NONE',  ( 3.330669073875469621E-13, -1.110223024625156540E-13, -2.999999999999971578 ) ) ;
#19188 = DIRECTION ( 'NONE',  ( 0.000000000000000000, -1.000000000000000000, 0.000000000000000000 ) ) ;
#19189 = ORIENTED_EDGE ( 'NONE', *, *, #21612, .T. ) ;
#19190 = DIRECTION ( 'NONE',  ( 0.000000000000000000, 0.000000000000000000, -1.000000000000000000 ) ) ;
#19191 = DIRECTION ( 'NONE',  ( 0.000000000000000000, 0.000000000000000000, 1.000000000000000000 ) ) ;
#19192 = VERTEX_POINT ( 'NONE', #1292 ) ;
#19193 = DIRECTION ( 'NONE',  ( 0.000000000000000000, 0.000000000000000000, 1.000000000000000000 ) ) ;
#19194 = EDGE_CURVE ( 'NONE', #1286, #21483, #21145, .T. ) ;
#19195 = ORIENTED_EDGE ( 'NONE', *, *, #13226, .T. ) ;
#19196 = DIRECTION ( 'NONE',  ( 0.000000000000000000, 1.000000000000000000, 0.000000000000000000 ) ) ;
#19197 = DIRECTION ( 'NONE',  ( -0.000000000000000000, -0.000000000000000000, 1.000000000000000000 ) ) ;
#19198 = CARTESIAN_POINT ( 'NONE',  ( -1.529841668203881122, 39.98623406166607452, 49.88755235896857698 ) ) ;
#19199 = CIRCLE ( 'NONE', #5629, 2.499999999999998668 ) ;
#19200 = CARTESIAN_POINT ( 'NONE',  ( -3.591923118226331086E-15, -5.000000000000000000, -44.98888751680799203 ) ) ;
#19201 = PLANE ( 'NONE',  #13248 ) ;
#19202 = ADVANCED_FACE ( 'NONE', ( #1411 ), #4854, .T. ) ;
#19203 = CARTESIAN_POINT ( 'NONE',  ( -27.19760187735867518, -24.73600648735113694, -2.800654218530429507 ) ) ;
#19204 = AXIS2_PLACEMENT_3D ( 'NONE', #9774, #20544, #3124 ) ;
#19205 = ORIENTED_EDGE ( 'NONE', *, *, #6633, .T. ) ;
#19206 = EDGE_CURVE ( 'NONE', #2199, #5004, #15927, .T. ) ;
#19207 = ORIENTED_EDGE ( 'NONE', *, *, #2962, .F. ) ;
#19208 = ORIENTED_EDGE ( 'NONE', *, *, #2984, .T. ) ;
#19209 = AXIS2_PLACEMENT_3D ( 'NONE', #328, #16121, #7319 ) ;
#19210 = ORIENTED_EDGE ( 'NONE', *, *, #5601, .T. ) ;
#19211 = LINE ( 'NONE', #17134, #12521 ) ;
#19212 = DIRECTION ( 'NONE',  ( -1.000000000000000000, -5.332156527697367955E-15, 0.000000000000000000 ) ) ;
#19213 = DIRECTION ( 'NONE',  ( 1.296372316667914327E-16, 1.000000000000000000, -0.000000000000000000 ) ) ;
#19214 = CARTESIAN_POINT ( 'NONE',  ( -34.99999999999980815, 40.00000000000000711, 52.47499999999922693 ) ) ;
#19215 = CARTESIAN_POINT ( 'NONE',  ( 6.501355124432292243, 39.72712729196061332, 53.07780958417031769 ) ) ;
#19216 = VERTEX_POINT ( 'NONE', #8738 ) ;
#19217 = CLOSED_SHELL ( 'NONE', ( #22568, #1607, #10101, #2879, #21621, #6076, #5223, #16189, #16473, #6805, #6549, #14470, #7183, #16845, #14369, #855, #14816, #17723, #10712, #3482, #6107, #2070, #11510, #18452, #7197, #4010, #16454, #17115, #17659, #19202, #4841, #20611, #9678, #8774, #22414, #17702, #11007, #11890, #565, #8685, #807, #5820, #5245, #1632, #19876, #11568, #17556, #5924, #7056, #13108, #13059, #16054, #19819, #15707, #11060 ) ) ;
#19218 = CARTESIAN_POINT ( 'NONE',  ( -35.00000000000000000, 0.000000000000000000, 1.387778780781445676E-14 ) ) ;
#19219 = CARTESIAN_POINT ( 'NONE',  ( 13.00000000000024336, -2.516660498395250745, -100.0000000000000000 ) ) ;
#19220 = CARTESIAN_POINT ( 'NONE',  ( 33.51030287062373247, 15.12081897056669000, -2.800654218530485018 ) ) ;
#19221 = DIRECTION ( 'NONE',  ( 0.000000000000000000, 0.000000000000000000, 1.000000000000000000 ) ) ;
#19222 = ORIENTED_EDGE ( 'NONE', *, *, #8808, .F. ) ;
#19223 = CARTESIAN_POINT ( 'NONE',  ( -16.96028156848957025, 30.61033039275980627, 59.80781543853676396 ) ) ;
#19224 = EDGE_CURVE ( 'NONE', #15616, #20003, #5515, .T. ) ;
#19225 = CARTESIAN_POINT ( 'NONE',  ( 28.49999999999998224, 19.99999999999999645, -105.0000000000000142 ) ) ;
#19226 = FACE_OUTER_BOUND ( 'NONE', #11979, .T. ) ;
#19227 = VECTOR ( 'NONE', #3366, 1000.000000000000000 ) ;
#19228 = ORIENTED_EDGE ( 'NONE', *, *, #4145, .F. ) ;
#19229 = EDGE_CURVE ( 'NONE', #3930, #7098, #2080, .T. ) ;
#19230 = CIRCLE ( 'NONE', #14069, 17.00000000000000711 ) ;
#19231 = B_SPLINE_CURVE_WITH_KNOTS ( 'NONE', 3,
 ( #22692, #12558, #1924, #3546, #1706, #17617, #6979, #9140, #194, #15667, #19461, #8907, #13934, #3764, #19121, #7189, #15881 ),
 .UNSPECIFIED., .F., .F.,
 ( 4, 1, 1, 2, 2, 1, 1, 1, 2, 2, 4 ),
 ( 0.000000000000000000, 0.1250000000000120182, 0.1875000000000164313, 0.2187500000000176803, 0.2500000000000188738, 0.3750000000000237588, 0.4375000000000262568, 0.4687500000000264788, 0.4843750000000252021, 0.5000000000000238698, 1.000000000000000000 ),
 .UNSPECIFIED. ) ;
#19232 = ORIENTED_EDGE ( 'NONE', *, *, #17504, .F. ) ;
#19233 = ORIENTED_EDGE ( 'NONE', *, *, #19563, .F. ) ;
#19234 = CIRCLE ( 'NONE', #22165, 0.9999999999999956701 ) ;
#19235 = CARTESIAN_POINT ( 'NONE',  ( 0.2227364088701092593, -1.232651810761194122, -48.42315971483877490 ) ) ;
#19236 = CARTESIAN_POINT ( 'NONE',  ( -33.51030287062373247, -15.12081897056669000, -2.800654218530457484 ) ) ;
#19237 = ORIENTED_EDGE ( 'NONE', *, *, #19406, .T. ) ;
#19238 = PLANE ( 'NONE',  #14997 ) ;
#19239 = ADVANCED_FACE ( 'NONE', ( #466 ), #14318, .T. ) ;
#19240 = LINE ( 'NONE', #10508, #12301 ) ;
#19241 = DIRECTION ( 'NONE',  ( 6.505213034913038160E-19, 3.903127820947822896E-18, 1.000000000000000000 ) ) ;
#19242 = AXIS2_PLACEMENT_3D ( 'NONE', #12942, #20181, #4487 ) ;
#19243 = CARTESIAN_POINT ( 'NONE',  ( -19.38379237384221554, 24.94684328524662575, -57.98195591854480568 ) ) ;
#19244 = VECTOR ( 'NONE', #14256, 1000.000000000000114 ) ;
#19245 = CARTESIAN_POINT ( 'NONE',  ( 28.52469787935785561, 10.00000000000000000, 4.095854054471903538 ) ) ;
#19246 = CIRCLE ( 'NONE', #3888, 34.90673715956759082 ) ;
#19247 = EDGE_LOOP ( 'NONE', ( #18964, #3616, #1095, #21058 ) ) ;
#19248 = DIRECTION ( 'NONE',  ( 0.000000000000000000, 1.000000000000000000, 0.000000000000000000 ) ) ;
#19249 = DIRECTION ( 'NONE',  ( 1.000000000000000000, 1.208970125616063028E-17, 0.000000000000000000 ) ) ;
#19250 = CIRCLE ( 'NONE', #4249, 19.11328065563151668 ) ;
#19251 = CARTESIAN_POINT ( 'NONE',  ( -35.00000000000000000, -4.999999999999997335, 57.00000000000003553 ) ) ;
#19252 = EDGE_CURVE ( 'NONE', #13545, #2882, #11637, .T. ) ;
#19253 = CARTESIAN_POINT ( 'NONE',  ( 14.05436202270909796, 14.70285576532228511, -45.40204559108964588 ) ) ;
#19254 = AXIS2_PLACEMENT_3D ( 'NONE', #12544, #2020, #15987 ) ;
#19255 = VERTEX_POINT ( 'NONE', #12277 ) ;
#19256 = CARTESIAN_POINT ( 'NONE',  ( 0.000000000000000000, -1.500000000000015099, 0.000000000000000000 ) ) ;
#19257 = CARTESIAN_POINT ( 'NONE',  ( 22.22891329980558695, -23.65408649739134006, -6.999999999999999112 ) ) ;
#19258 = AXIS2_PLACEMENT_3D ( 'NONE', #5462, #15761, #12326 ) ;
#19259 = ORIENTED_EDGE ( 'NONE', *, *, #19705, .T. ) ;
#19260 = AXIS2_PLACEMENT_3D ( 'NONE', #7603, #16767, #16650 ) ;
#19261 = AXIS2_PLACEMENT_3D ( 'NONE', #8815, #8702, #12139 ) ;
#19262 = ORIENTED_EDGE ( 'NONE', *, *, #3060, .T. ) ;
#19263 = CARTESIAN_POINT ( 'NONE',  ( -0.7857880201000499998, 25.00083595504925071, 7.000278651543347053 ) ) ;
#19264 = VECTOR ( 'NONE', #20947, 1000.000000000000000 ) ;
#19265 = CARTESIAN_POINT ( 'NONE',  ( 2.419767991120476136, -3.149022461038316845, 49.02154318835460600 ) ) ;
#19266 = DIRECTION ( 'NONE',  ( 0.000000000000000000, 1.000000000000000000, -0.000000000000000000 ) ) ;
#19267 = CARTESIAN_POINT ( 'NONE',  ( -5.833333333333325932, 40.00000000000000000, 40.61164310337068883 ) ) ;
#19268 = ADVANCED_FACE ( 'NONE', ( #17433 ), #5624, .F. ) ;
#19269 = DIRECTION ( 'NONE',  ( 6.505213034913038160E-19, 3.903127820947822896E-18, 1.000000000000000000 ) ) ;
#19270 = ORIENTED_EDGE ( 'NONE', *, *, #12907, .F. ) ;
#19271 = DIRECTION ( 'NONE',  ( -1.000000000000000000, 1.296372316667914327E-16, 0.000000000000000000 ) ) ;
#19272 = DIRECTION ( 'NONE',  ( -0.000000000000000000, 1.000000000000000000, -0.000000000000000000 ) ) ;
#19273 = ORIENTED_EDGE ( 'NONE', *, *, #8080, .F. ) ;
#19274 = CARTESIAN_POINT ( 'NONE',  ( 4.170748987303435129, -34.65667543218869895, 2.999999999999999112 ) ) ;
#19275 = DIRECTION ( 'NONE',  ( 0.000000000000000000, 0.000000000000000000, 1.000000000000000000 ) ) ;
#19276 = CARTESIAN_POINT ( 'NONE',  ( -15.49999999999980282, -2.516660498395516310, -100.0000000000000000 ) ) ;
#19277 = CYLINDRICAL_SURFACE ( 'NONE', #17819, 22.12933039895921539 ) ;
#19278 = CARTESIAN_POINT ( 'NONE',  ( -9.506747391179116491, 40.00000000000000711, -53.50938557766276915 ) ) ;
#19279 = ORIENTED_EDGE ( 'NONE', *, *, #7502, .F. ) ;
#19280 = DIRECTION ( 'NONE',  ( -6.505213034913038160E-19, -3.903127820947822896E-18, -1.000000000000000000 ) ) ;
#19281 = EDGE_CURVE ( 'NONE', #11262, #11081, #9073, .T. ) ;
#19282 = EDGE_CURVE ( 'NONE', #19871, #10716, #20070, .T. ) ;
#19283 = CARTESIAN_POINT ( 'NONE',  ( -15.92429324705536864, 4.173694850190172723, 56.88791232810483933 ) ) ;
#19284 = AXIS2_PLACEMENT_3D ( 'NONE', #9293, #13044, #18106 ) ;
#19285 = EDGE_CURVE ( 'NONE', #18296, #5024, #18979, .T. ) ;
#19286 = VERTEX_POINT ( 'NONE', #14774 ) ;
#19287 = CARTESIAN_POINT ( 'NONE',  ( 1.102182119232617517E-15, 0.000000000000000000, 8.999999999999998224 ) ) ;
#19288 = FACE_BOUND ( 'NONE', #10216, .T. ) ;
#19289 = EDGE_CURVE ( 'NONE', #8759, #3548, #17125, .T. ) ;
#19290 = CIRCLE ( 'NONE', #13394, 2.099999999999990763 ) ;
#19291 = EDGE_CURVE ( 'NONE', #21584, #10900, #14881, .T. ) ;
#19292 = VERTEX_POINT ( 'NONE', #7691 ) ;
#19293 = VERTEX_POINT ( 'NONE', #4484 ) ;
#19294 = ORIENTED_EDGE ( 'NONE', *, *, #12158, .F. ) ;
#19295 = ORIENTED_EDGE ( 'NONE', *, *, #3309, .T. ) ;
#19296 = DIRECTION ( 'NONE',  ( -1.000000000000000000, -1.208970125616062874E-17, 0.000000000000000000 ) ) ;
#19297 = CYLINDRICAL_SURFACE ( 'NONE', #18800, 36.76383501243555685 ) ;
#19298 = DIRECTION ( 'NONE',  ( -0.000000000000000000, -1.000000000000000000, -0.000000000000000000 ) ) ;
#19299 = DIRECTION ( 'NONE',  ( 1.000000000000000000, 0.000000000000000000, 0.000000000000000000 ) ) ;
#19300 = EDGE_LOOP ( 'NONE', ( #16615, #4645, #19729, #21763 ) ) ;
#19301 = DIRECTION ( 'NONE',  ( 0.000000000000000000, 0.000000000000000000, 1.000000000000000000 ) ) ;
#19302 = DIRECTION ( 'NONE',  ( -0.1421319796954322034, 0.000000000000000000, -0.9898477157360405787 ) ) ;
#19303 = ORIENTED_EDGE ( 'NONE', *, *, #21280, .T. ) ;
#19304 = CARTESIAN_POINT ( 'NONE',  ( -8.349099696861312481, 1.803277857259543593, 53.93591755799874221 ) ) ;
#19305 = B_SPLINE_CURVE_WITH_KNOTS ( 'NONE', 3,
 ( #13558, #10018, #18635, #2940 ),
 .UNSPECIFIED., .F., .F.,
 ( 4, 4 ),
 ( 9.715086428218796083E-07, 0.001929643240674198870 ),
 .UNSPECIFIED. ) ;
#19306 = CARTESIAN_POINT ( 'NONE',  ( -10.27431133777640149, -4.928932188134504955, 51.43682631505699732 ) ) ;
#19307 = EDGE_LOOP ( 'NONE', ( #20833, #14588, #1168, #5098 ) ) ;
#19308 = DIRECTION ( 'NONE',  ( 1.000000000000000000, 0.000000000000000000, 0.000000000000000000 ) ) ;
#19309 = ORIENTED_EDGE ( 'NONE', *, *, #10883, .F. ) ;
#19310 = CARTESIAN_POINT ( 'NONE',  ( -2.278855561005702801E-14, 40.00000000000000000, -48.73397172404479250 ) ) ;
#19311 = CARTESIAN_POINT ( 'NONE',  ( 1.387778780781445676E-14, 40.00000000000000000, 48.73397172404482802 ) ) ;
#19312 = CARTESIAN_POINT ( 'NONE',  ( -0.5525077609812600876, 39.99819305627858057, 49.15917909279997389 ) ) ;
#19313 = VECTOR ( 'NONE', #19073, 1000.000000000000000 ) ;
#19314 = CIRCLE ( 'NONE', #10862, 34.90673715956759082 ) ;
#19315 = CARTESIAN_POINT ( 'NONE',  ( 22.38103533145805102, 18.35979201191610244, 58.65801380639354790 ) ) ;
#19316 = LINE ( 'NONE', #3506, #7062 ) ;
#19317 = AXIS2_PLACEMENT_3D ( 'NONE', #7300, #5487, #12456 ) ;
#19318 = ADVANCED_FACE ( 'NONE', ( #14668 ), #18230, .T. ) ;
#19319 = EDGE_CURVE ( 'NONE', #13976, #18872, #5425, .T. ) ;
#19320 = DIRECTION ( 'NONE',  ( -1.000000000000000000, 0.000000000000000000, 0.000000000000000000 ) ) ;
#19321 = ORIENTED_EDGE ( 'NONE', *, *, #21221, .F. ) ;
#19322 = AXIS2_PLACEMENT_3D ( 'NONE', #20102, #14589, #11151 ) ;
#19323 = EDGE_CURVE ( 'NONE', #6092, #5279, #8252, .T. ) ;
#19324 = CIRCLE ( 'NONE', #6280, 36.76383501243555685 ) ;
#19325 = ORIENTED_EDGE ( 'NONE', *, *, #12490, .T. ) ;
#19326 = EDGE_LOOP ( 'NONE', ( #9866, #19063, #12032, #12494 ) ) ;
#19327 = DIRECTION ( 'NONE',  ( -0.000000000000000000, 1.000000000000000000, -0.000000000000000000 ) ) ;
#19328 = CARTESIAN_POINT ( 'NONE',  ( -42.50000000000000000, 10.00000000000000000, 47.49999999999999289 ) ) ;
#19329 = VECTOR ( 'NONE', #89, 1000.000000000000000 ) ;
#19330 = CIRCLE ( 'NONE', #12355, 31.50000000000000711 ) ;
#19331 = LINE ( 'NONE', #3638, #17510 ) ;
#19332 = DIRECTION ( 'NONE',  ( -6.505213034913038160E-19, -3.903127820947822896E-18, -1.000000000000000000 ) ) ;
#19333 = CARTESIAN_POINT ( 'NONE',  ( 0.5323810940973144890, 39.99832332085551201, 49.14386465755924149 ) ) ;
#19334 = ORIENTED_EDGE ( 'NONE', *, *, #3932, .F. ) ;
#19335 = FACE_OUTER_BOUND ( 'NONE', #18460, .T. ) ;
#19336 = CARTESIAN_POINT ( 'NONE',  ( 22.26748298433264850, -22.28024240313505899, -2.999999999999971578 ) ) ;
#19337 = CARTESIAN_POINT ( 'NONE',  ( 7.943521403985130338E-15, 0.000000000000000000, -47.49736834814795827 ) ) ;
#19338 = DIRECTION ( 'NONE',  ( -1.000000000000000000, -1.208970125616060101E-17, 6.505213034913038160E-19 ) ) ;
#19339 = FACE_OUTER_BOUND ( 'NONE', #16532, .T. ) ;
#19340 = EDGE_CURVE ( 'NONE', #6067, #4414, #10069, .T. ) ;
#19341 = CIRCLE ( 'NONE', #8349, 36.76383501243555685 ) ;
#19342 = SURFACE_STYLE_USAGE ( .BOTH. , #19452 ) ;
#19343 = AXIS2_PLACEMENT_3D ( 'NONE', #7036, #8974, #19308 ) ;
#19344 = CARTESIAN_POINT ( 'NONE',  ( -6.433485051968491852, 38.94088993357631523, 55.16018527339316080 ) ) ;
#19345 = DIRECTION ( 'NONE',  ( 0.000000000000000000, 0.000000000000000000, 1.000000000000000000 ) ) ;
#19346 = VECTOR ( 'NONE', #2710, 1000.000000000000000 ) ;
#19347 = CARTESIAN_POINT ( 'NONE',  ( 42.50000000000000000, 10.00000000000000000, 47.49999999999999289 ) ) ;
#19348 = VECTOR ( 'NONE', #8999, 1000.000000000000000 ) ;
#19349 = VERTEX_POINT ( 'NONE', #4118 ) ;
#19350 = ORIENTED_EDGE ( 'NONE', *, *, #16805, .F. ) ;
#19351 = VERTEX_POINT ( 'NONE', #21879 ) ;
#19352 = CARTESIAN_POINT ( 'NONE',  ( 31.67162468656012209, 14.67611967928900185, -2.999999999999971578 ) ) ;
#19353 = AXIS2_PLACEMENT_3D ( 'NONE', #22091, #9826, #9170 ) ;
#19354 = VECTOR ( 'NONE', #4948, 1000.000000000000000 ) ;
#19355 = DIRECTION ( 'NONE',  ( -0.000000000000000000, -1.000000000000000000, -0.000000000000000000 ) ) ;
#19356 = EDGE_CURVE ( 'NONE', #14756, #15733, #11277, .T. ) ;
#19357 = VECTOR ( 'NONE', #5128, 1000.000000000000000 ) ;
#19358 = VECTOR ( 'NONE', #2913, 1000.000000000000000 ) ;
#19359 = DIRECTION ( 'NONE',  ( 0.000000000000000000, 0.000000000000000000, 1.000000000000000000 ) ) ;
#19360 = CARTESIAN_POINT ( 'NONE',  ( 35.00000000000001421, 4.000000000000028422, -10.00000000000000000 ) ) ;
#19361 = CARTESIAN_POINT ( 'NONE',  ( 42.50000000000000711, -12.00000000000012434, 50.02500000000011937 ) ) ;
#19362 = CARTESIAN_POINT ( 'NONE',  ( -17.16827611621724969, 34.47540479398168856, -57.28984973304980599 ) ) ;
#19363 = VECTOR ( 'NONE', #22374, 1000.000000000000000 ) ;
#19364 = DIRECTION ( 'NONE',  ( 0.000000000000000000, -1.000000000000000000, 0.000000000000000000 ) ) ;
#19365 = EDGE_CURVE ( 'NONE', #3635, #5980, #14406, .T. ) ;
#19366 = EDGE_LOOP ( 'NONE', ( #58, #3562 ) ) ;
#19367 = LINE ( 'NONE', #6987, #18931 ) ;
#19368 = LINE ( 'NONE', #2390, #15465 ) ;
#19369 = FACE_BOUND ( 'NONE', #15926, .T. ) ;
#19370 = CARTESIAN_POINT ( 'NONE',  ( 14.99999999999998579, 19.22713695939443568, -45.82575694955836809 ) ) ;
#19371 = VERTEX_POINT ( 'NONE', #12910 ) ;
#19372 = AXIS2_PLACEMENT_3D ( 'NONE', #18192, #5354, #13691 ) ;
#19373 = DIRECTION ( 'NONE',  ( -1.000000000000000000, -2.486827044406942538E-14, 0.000000000000000000 ) ) ;
#19374 = CARTESIAN_POINT ( 'NONE',  ( -35.00000000000000000, 2.142135623730931471, 1.387778780781445676E-14 ) ) ;
#19375 = CIRCLE ( 'NONE', #21194, 3.999999999999998224 ) ;
#19376 = ADVANCED_FACE ( 'NONE', ( #4460 ), #556, .F. ) ;
#19377 = EDGE_LOOP ( 'NONE', ( #3990, #5527, #21144, #3656, #8932, #17313, #1225 ) ) ;
#19378 = EDGE_CURVE ( 'NONE', #22383, #7, #4230, .T. ) ;
#19379 = VERTEX_POINT ( 'NONE', #4352 ) ;
#19380 = CARTESIAN_POINT ( 'NONE',  ( 0.1620509895534447964, 39.99984822922976946, -48.85971511756937247 ) ) ;
#19381 = DIRECTION ( 'NONE',  ( -0.000000000000000000, -1.000000000000000000, -0.000000000000000000 ) ) ;
#19382 =( GEOMETRIC_REPRESENTATION_CONTEXT ( 3 ) GLOBAL_UNCERTAINTY_ASSIGNED_CONTEXT ( ( #8069 ) ) GLOBAL_UNIT_ASSIGNED_CONTEXT ( ( #3672, #9035, #15895 ) ) REPRESENTATION_CONTEXT ( 'NONE', 'WORKASPACE' ) );
#19383 = CARTESIAN_POINT ( 'NONE',  ( -10.49999999999980282, -2.516660498395516310, 105.0000000000000142 ) ) ;
#19384 = ORIENTED_EDGE ( 'NONE', *, *, #15572, .F. ) ;
#19385 = CARTESIAN_POINT ( 'NONE',  ( -34.99999999999999289, 40.00000000000000000, -51.00000000000000711 ) ) ;
#19386 = CARTESIAN_POINT ( 'NONE',  ( -9.952189117650803496, 40.00000000000000000, 53.64426396172073908 ) ) ;
#19387 = ORIENTED_EDGE ( 'NONE', *, *, #19534, .F. ) ;
#19388 = DIRECTION ( 'NONE',  ( -0.000000000000000000, -0.000000000000000000, 1.000000000000000000 ) ) ;
#19389 = FACE_OUTER_BOUND ( 'NONE', #16098, .T. ) ;
#19390 = DIRECTION ( 'NONE',  ( 6.505213034913038160E-19, 3.903127820947822896E-18, 1.000000000000000000 ) ) ;
#19391 = DIRECTION ( 'NONE',  ( -1.000000000000000000, 4.350865286404990634E-14, 0.000000000000000000 ) ) ;
#19392 = ORIENTED_EDGE ( 'NONE', *, *, #2889, .T. ) ;
#19393 = DIRECTION ( 'NONE',  ( 0.000000000000000000, 1.000000000000000000, 0.000000000000000000 ) ) ;
#19394 = CARTESIAN_POINT ( 'NONE',  ( 33.46652738560686657, -11.93772187171692245, -2.999999999999998224 ) ) ;
#19395 = CARTESIAN_POINT ( 'NONE',  ( -2.244030815477592533, 39.96966515101875217, -50.39883272053734231 ) ) ;
#19396 = ORIENTED_EDGE ( 'NONE', *, *, #4758, .F. ) ;
#19397 = CARTESIAN_POINT ( 'NONE',  ( 11.68090480754630001, 3.765577839755386957, 57.90797000640142755 ) ) ;
#19398 = DIRECTION ( 'NONE',  ( 0.000000000000000000, 0.000000000000000000, 1.000000000000000000 ) ) ;
#19399 = CARTESIAN_POINT ( 'NONE',  ( 35.00000000000001421, 4.000000000000028422, 1.540743955509788682E-30 ) ) ;
#19400 = ADVANCED_FACE ( 'NONE', ( #17972, #11329, #7666, #18313, #2632 ), #16589, .T. ) ;
#19401 = COLOUR_RGB ( '',0.7921568627450980005, 0.8196078431372548767, 0.9333333333333333481 ) ;
#19402 = ORIENTED_EDGE ( 'NONE', *, *, #4105, .T. ) ;
#19403 = ORIENTED_EDGE ( 'NONE', *, *, #2232, .F. ) ;
#19404 = VERTEX_POINT ( 'NONE', #899 ) ;
#19405 = EDGE_CURVE ( 'NONE', #14751, #14834, #13094, .T. ) ;
#19406 = EDGE_CURVE ( 'NONE', #31, #14783, #19341, .T. ) ;
#19407 = ADVANCED_FACE ( 'NONE', ( #11666 ), #7617, .F. ) ;
#19408 = VERTEX_POINT ( 'NONE', #13697 ) ;
#19409 = DIRECTION ( 'NONE',  ( 0.000000000000000000, 1.000000000000000000, 0.000000000000000000 ) ) ;
#19410 = CARTESIAN_POINT ( 'NONE',  ( 15.37127427991059392, 36.37761751580015357, 56.70227746889294451 ) ) ;
#19411 = AXIS2_PLACEMENT_3D ( 'NONE', #19597, #19266, #17639 ) ;
#19412 = CARTESIAN_POINT ( 'NONE',  ( 9.454383690904577975, 39.37264121342599310, -54.46710214104096792 ) ) ;
#19413 = CARTESIAN_POINT ( 'NONE',  ( 9.193775052642715551, 40.00000000000000711, 53.40447181116137898 ) ) ;
#19414 = ORIENTED_EDGE ( 'NONE', *, *, #19588, .T. ) ;
#19415 = CARTESIAN_POINT ( 'NONE',  ( -1.387778780781445518E-14, 20.00000000000000355, 105.0000000000000142 ) ) ;
#19416 = CARTESIAN_POINT ( 'NONE',  ( 6.696867368504048330E-15, 5.000000000000000888, 38.73397172404480671 ) ) ;
#19417 = ORIENTED_EDGE ( 'NONE', *, *, #10148, .F. ) ;
#19418 = CARTESIAN_POINT ( 'NONE',  ( 0.8615617109688762376, 36.14854559161343417, -2.932164912090547748 ) ) ;
#19419 = DIRECTION ( 'NONE',  ( -1.000000000000000000, -1.208970125616044077E-17, 0.000000000000000000 ) ) ;
#19420 = CARTESIAN_POINT ( 'NONE',  ( 3.071904583821672593E-15, -4.500000000000010658, 0.000000000000000000 ) ) ;
#19421 = VERTEX_POINT ( 'NONE', #22439 ) ;
#19422 = CARTESIAN_POINT ( 'NONE',  ( 6.976853941385730451, 1.175947842330679061, 53.23020196600168674 ) ) ;
#19423 = ORIENTED_EDGE ( 'NONE', *, *, #18615, .F. ) ;
#19424 = DIRECTION ( 'NONE',  ( -1.000000000000000000, -1.208970125616046080E-17, 6.505213034913038160E-19 ) ) ;
#19425 = EDGE_CURVE ( 'NONE', #22614, #3371, #22216, .T. ) ;
#19426 = CARTESIAN_POINT ( 'NONE',  ( -0.1539325450100966219, 40.00000000000000711, 48.91834387730083478 ) ) ;
#19427 = CARTESIAN_POINT ( 'NONE',  ( 42.50000000000000711, -11.97499999999999964, 45.00000000000000711 ) ) ;
#19428 = FILL_AREA_STYLE ('',( #5441 ) ) ;
#19429 = CARTESIAN_POINT ( 'NONE',  ( 19.42731605662046235, 15.16896271047388822, 57.99434643147303348 ) ) ;
#19430 = AXIS2_PLACEMENT_3D ( 'NONE', #21179, #7418, #5480 ) ;
#19431 = DIRECTION ( 'NONE',  ( 1.000000000000000000, 0.000000000000000000, 0.000000000000000000 ) ) ;
#19432 = EDGE_CURVE ( 'NONE', #12412, #12073, #16394, .T. ) ;
#19433 = EDGE_LOOP ( 'NONE', ( #1419, #12203, #13324, #20567 ) ) ;
#19434 = VERTEX_POINT ( 'NONE', #20715 ) ;
#19435 = VERTEX_POINT ( 'NONE', #1349 ) ;
#19436 = EDGE_LOOP ( 'NONE', ( #3724, #18912, #8415, #14011, #18844, #22020, #15134 ) ) ;
#19437 = DIRECTION ( 'NONE',  ( -0.9898477157360405787, 0.000000000000000000, -0.1421319796954322312 ) ) ;
#19438 = CARTESIAN_POINT ( 'NONE',  ( 2.775557561562891351E-14, -2.775557561562891351E-14, 2.999999999999999112 ) ) ;
#19439 = FACE_OUTER_BOUND ( 'NONE', #3642, .T. ) ;
#19440 = CARTESIAN_POINT ( 'NONE',  ( -13.00000000000000178, -20.00000000000000000, -11.32475165290611407 ) ) ;
#19441 = CARTESIAN_POINT ( 'NONE',  ( -26.64365646977254087, -17.09029715894938661, 3.000000000000012879 ) ) ;
#19442 = CARTESIAN_POINT ( 'NONE',  ( 0.01336081163439876984, 39.99999903713349880, 48.74437065933960156 ) ) ;
#19443 = ADVANCED_FACE ( 'NONE', ( #3191 ), #18602, .T. ) ;
#19444 = AXIS2_PLACEMENT_3D ( 'NONE', #21684, #2778, #13400 ) ;
#19445 = EDGE_CURVE ( 'NONE', #16838, #8405, #6619, .T. ) ;
#19446 = VERTEX_POINT ( 'NONE', #13819 ) ;
#19447 = CARTESIAN_POINT ( 'NONE',  ( 12.82970538955578022, 1.687462484003134255, -55.75926248610264224 ) ) ;
#19448 = CARTESIAN_POINT ( 'NONE',  ( 0.6841746959068695233, 36.75746821813305587, 2.800654218530485018 ) ) ;
#19449 = DIRECTION ( 'NONE',  ( 0.000000000000000000, -0.7071067811865500152, 0.7071067811865451302 ) ) ;
#19450 = CARTESIAN_POINT ( 'NONE',  ( 4.683984772515712893E-15, 0.6398376396478597794, -17.00000000000000711 ) ) ;
#19451 = ADVANCED_FACE ( 'NONE', ( #3312 ), #10493, .F. ) ;
#19452 = SURFACE_SIDE_STYLE ('',( #12112 ) ) ;
#19453 = AXIS2_PLACEMENT_3D ( 'NONE', #3057, #4673, #6379 ) ;
#19454 = DIRECTION ( 'NONE',  ( -1.000000000000000000, 1.301042606982605814E-16, 0.000000000000000000 ) ) ;
#19455 = DIRECTION ( 'NONE',  ( -0.000000000000000000, -0.000000000000000000, 1.000000000000000000 ) ) ;
#19456 = ORIENTED_EDGE ( 'NONE', *, *, #4962, .T. ) ;
#19457 = ORIENTED_EDGE ( 'NONE', *, *, #11414, .F. ) ;
#19458 = B_SPLINE_CURVE_WITH_KNOTS ( 'NONE', 3,
 ( #4679, #13010, #11542, #20374 ),
 .UNSPECIFIED., .F., .F.,
 ( 4, 4 ),
 ( 0.001875451646902865028, 0.003761979286331341814 ),
 .UNSPECIFIED. ) ;
#19459 = ORIENTED_EDGE ( 'NONE', *, *, #21113, .T. ) ;
#19460 = CARTESIAN_POINT ( 'NONE',  ( 0.7217013448888215388, -4.626342591370756985, -46.01887142925446739 ) ) ;
#19461 = CARTESIAN_POINT ( 'NONE',  ( 11.19713514086473438, 39.99999999999999289, -54.03748032825708236 ) ) ;
#19462 = DIRECTION ( 'NONE',  ( -1.000000000000000000, -1.208970125616060101E-17, 6.505213034913038160E-19 ) ) ;
#19463 = CARTESIAN_POINT ( 'NONE',  ( -48.93401015228426587, 7.000000000000000000, 46.57614213197968667 ) ) ;
#19464 = CARTESIAN_POINT ( 'NONE',  ( -90.00000000000000000, 40.00000000000000000, 2.099999999999989875 ) ) ;
#19465 = CARTESIAN_POINT ( 'NONE',  ( -13.09671971564483073, 38.20119746052779419, -55.86054988736573534 ) ) ;
#19466 = CARTESIAN_POINT ( 'NONE',  ( -27.64365646977265456, -17.09029715894952517, -2.999999999999981792 ) ) ;
#19467 = ADVANCED_BREP_SHAPE_REPRESENTATION ( '', ( #18090, #18273 ), #12407 ) ;
#19468 = ORIENTED_EDGE ( 'NONE', *, *, #12096, .T. ) ;
#19469 = FACE_OUTER_BOUND ( 'NONE', #7842, .T. ) ;
#19470 = DIRECTION ( 'NONE',  ( -1.000000000000000000, 1.084202172485505420E-16, 0.000000000000000000 ) ) ;
#19471 = FACE_BOUND ( 'NONE', #7869, .T. ) ;
#19472 = CARTESIAN_POINT ( 'NONE',  ( 9.579024991657044907, 8.451577327321118105, -43.05667825653225123 ) ) ;
#19473 = ORIENTED_EDGE ( 'NONE', *, *, #2852, .T. ) ;
#19474 = CARTESIAN_POINT ( 'NONE',  ( -13.83143812983099430, 29.36548507648012318, -7.000000000000006217 ) ) ;
#19475 = DIRECTION ( 'NONE',  ( 0.000000000000000000, 0.000000000000000000, 1.000000000000000000 ) ) ;
#19476 = ADVANCED_FACE ( 'NONE', ( #14146 ), #22682, .F. ) ;
#19477 = DIRECTION ( 'NONE',  ( -0.000000000000000000, -1.000000000000000000, -0.000000000000000000 ) ) ;
#19478 = AXIS2_PLACEMENT_3D ( 'NONE', #12318, #10590, #3636 ) ;
#19479 = ORIENTED_EDGE ( 'NONE', *, *, #7341, .T. ) ;
#19480 = ADVANCED_FACE ( 'NONE', ( #1695, #3650 ), #21052, .T. ) ;
#19481 = ORIENTED_EDGE ( 'NONE', *, *, #13504, .T. ) ;
#19482 = CARTESIAN_POINT ( 'NONE',  ( 0.04635509897966557519, 40.00000000000001421, -48.77005890240622676 ) ) ;
#19483 = CARTESIAN_POINT ( 'NONE',  ( 15.02862401740831544, 32.75570538720759828, 2.999999999999995559 ) ) ;
#19484 = CARTESIAN_POINT ( 'NONE',  ( 90.00000000000000000, 26.00000000000000355, 2.099999999999989875 ) ) ;
#19485 = CARTESIAN_POINT ( 'NONE',  ( 14.74639653023232455, -28.96193690644940943, -6.999999999999944045 ) ) ;
#19486 = VERTEX_POINT ( 'NONE', #9234 ) ;
#19487 = DIRECTION ( 'NONE',  ( -6.505213034913038160E-19, -3.903127820947822896E-18, -1.000000000000000000 ) ) ;
#19488 = CARTESIAN_POINT ( 'NONE',  ( -8.421829293842984399, 39.99999999999998579, 53.12761752185808461 ) ) ;
#19489 = ORIENTED_EDGE ( 'NONE', *, *, #8536, .T. ) ;
#19490 = FACE_OUTER_BOUND ( 'NONE', #10010, .T. ) ;
#19491 = CARTESIAN_POINT ( 'NONE',  ( 22.15746142094439719, 16.52917608750723488, -58.60949679988861050 ) ) ;
#19492 = CIRCLE ( 'NONE', #15807, 2.099999999999997868 ) ;
#19493 = AXIS2_PLACEMENT_3D ( 'NONE', #2811, #11732, #1303 ) ;
#19494 = CARTESIAN_POINT ( 'NONE',  ( 15.50000000000024336, -2.516660498395250301, -105.0000000000000142 ) ) ;
#19495 = ORIENTED_EDGE ( 'NONE', *, *, #14587, .F. ) ;
#19496 = CYLINDRICAL_SURFACE ( 'NONE', #14109, 5.000000000000000000 ) ;
#19497 = CARTESIAN_POINT ( 'NONE',  ( -10.31465995609392827, 2.846668092513518378, 57.27881138849647868 ) ) ;
#19498 = CARTESIAN_POINT ( 'NONE',  ( -6.718896912932006416, 39.70714865612620059, -53.19564684132798504 ) ) ;
#19499 = TOROIDAL_SURFACE ( 'NONE', #8163, 34.90673715956759082, 8.750000000000000000 ) ;
#19500 = ORIENTED_EDGE ( 'NONE', *, *, #8740, .F. ) ;
#19501 = CARTESIAN_POINT ( 'NONE',  ( -35.00000000000000000, 15.00000000000000000, 41.00000000000002132 ) ) ;
#19502 = DIRECTION ( 'NONE',  ( 0.000000000000000000, -1.000000000000000000, 0.000000000000000000 ) ) ;
#19503 = EDGE_CURVE ( 'NONE', #950, #19717, #16765, .T. ) ;
#19504 = ORIENTED_EDGE ( 'NONE', *, *, #2637, .F. ) ;
#19505 = EDGE_CURVE ( 'NONE', #12184, #15016, #19697, .T. ) ;
#19506 = CIRCLE ( 'NONE', #18772, 2.499999999999995115 ) ;
#19507 = ORIENTED_EDGE ( 'NONE', *, *, #15267, .T. ) ;
#19508 = VERTEX_POINT ( 'NONE', #11177 ) ;
#19509 = VECTOR ( 'NONE', #7239, 1000.000000000000000 ) ;
#19510 = ORIENTED_EDGE ( 'NONE', *, *, #11211, .F. ) ;
#19511 = LINE ( 'NONE', #5524, #6651 ) ;
#19512 = CARTESIAN_POINT ( 'NONE',  ( -35.00000000000000000, -5.000000000000000000, 1.387778780781445676E-14 ) ) ;
#19513 = DIRECTION ( 'NONE',  ( -6.505213034913038160E-19, -3.903127820947822896E-18, -1.000000000000000000 ) ) ;
#19514 = CARTESIAN_POINT ( 'NONE',  ( 0.000000000000000000, 30.00000000000000355, 4.025000000000000355 ) ) ;
#19515 = ORIENTED_EDGE ( 'NONE', *, *, #16066, .T. ) ;
#19516 = DIRECTION ( 'NONE',  ( -1.000000000000000000, 0.000000000000000000, 0.000000000000000000 ) ) ;
#19517 = DIRECTION ( 'NONE',  ( 6.505213034913038160E-19, 3.903127820947822896E-18, 1.000000000000000000 ) ) ;
#19518 = ORIENTED_EDGE ( 'NONE', *, *, #4668, .F. ) ;
#19519 = CARTESIAN_POINT ( 'NONE',  ( -14.14132741310376851, -16.85297774861785314, -4.999999999999955591 ) ) ;
#19520 = CARTESIAN_POINT ( 'NONE',  ( -15.37127427991062056, 36.37761751580014646, -56.70227746889291609 ) ) ;
#19521 = CARTESIAN_POINT ( 'NONE',  ( 36.06598984771573413, 10.00000000000000000, 48.42385786802029912 ) ) ;
#19522 = ORIENTED_EDGE ( 'NONE', *, *, #10857, .T. ) ;
#19523 = ADVANCED_FACE ( 'NONE', ( #16457 ), #15287, .T. ) ;
#19524 = FACE_OUTER_BOUND ( 'NONE', #6922, .T. ) ;
#19525 = EDGE_LOOP ( 'NONE', ( #16925, #11730, #10445, #15339 ) ) ;
#19526 = DIRECTION ( 'NONE',  ( -6.505213034913038160E-19, -3.903127820947822896E-18, -1.000000000000000000 ) ) ;
#19527 = CARTESIAN_POINT ( 'NONE',  ( 35.00000000000001421, 14.00000000000000000, 39.00000000000002132 ) ) ;
#19528 = CARTESIAN_POINT ( 'NONE',  ( -25.34312177887334983, 20.17230487860824439, -2.999999999999971578 ) ) ;
#19529 = FACE_OUTER_BOUND ( 'NONE', #10302, .T. ) ;
#19530 = DIRECTION ( 'NONE',  ( 6.505213034913038160E-19, 3.903127820947822896E-18, 1.000000000000000000 ) ) ;
#19531 = AXIS2_PLACEMENT_3D ( 'NONE', #11733, #18497, #13100 ) ;
#19532 = CARTESIAN_POINT ( 'NONE',  ( 19.67353980729958352, 23.69994786804610953, 58.06093965454051897 ) ) ;
#19533 = DIRECTION ( 'NONE',  ( 1.000000000000000000, 1.208970125616053784E-17, 0.000000000000000000 ) ) ;
#19534 = EDGE_CURVE ( 'NONE', #14442, #817, #12720, .T. ) ;
#19535 = EDGE_CURVE ( 'NONE', #6950, #10113, #7860, .T. ) ;
#19536 = AXIS2_PLACEMENT_3D ( 'NONE', #8707, #13950, #2 ) ;
#19537 = CARTESIAN_POINT ( 'NONE',  ( -16.99647590252638452, -30.48934413892778750, 2.999999999999999112 ) ) ;
#19538 = ORIENTED_EDGE ( 'NONE', *, *, #2720, .F. ) ;
#19539 = CIRCLE ( 'NONE', #4548, 3.999999999999999112 ) ;
#19540 = ORIENTED_EDGE ( 'NONE', *, *, #7770, .T. ) ;
#19541 = EDGE_CURVE ( 'NONE', #16891, #5024, #18976, .T. ) ;
#19542 = EDGE_LOOP ( 'NONE', ( #3633, #16088 ) ) ;
#19543 = B_SPLINE_CURVE_WITH_KNOTS ( 'NONE', 3,
 ( #2450, #5645, #14575, #12742 ),
 .UNSPECIFIED., .F., .F.,
 ( 4, 4 ),
 ( 9.715086412473486974E-07, 0.001929643240672463496 ),
 .UNSPECIFIED. ) ;
#19544 = ORIENTED_EDGE ( 'NONE', *, *, #3763, .F. ) ;
#19545 = DIRECTION ( 'NONE',  ( -0.000000000000000000, -1.000000000000000000, -0.000000000000000000 ) ) ;
#19546 = DIRECTION ( 'NONE',  ( 0.000000000000000000, 0.000000000000000000, -1.000000000000000000 ) ) ;
#19547 = DIRECTION ( 'NONE',  ( -0.000000000000000000, 1.000000000000000000, -0.000000000000000000 ) ) ;
#19548 = EDGE_CURVE ( 'NONE', #5940, #15936, #9456, .T. ) ;
#19549 = CARTESIAN_POINT ( 'NONE',  ( -22.22891329980540576, 23.65408649739122993, -7.000000000000006217 ) ) ;
#19550 = CARTESIAN_POINT ( 'NONE',  ( 6.687085176834780320, 39.71011800170725792, 53.17853448240479963 ) ) ;
#19551 = AXIS2_PLACEMENT_3D ( 'NONE', #8031, #14991, #20175 ) ;
#19552 = EDGE_CURVE ( 'NONE', #8421, #4768, #8708, .T. ) ;
#19553 = ORIENTED_EDGE ( 'NONE', *, *, #21083, .F. ) ;
#19554 = CARTESIAN_POINT ( 'NONE',  ( 42.50000000000000711, -12.00000000000000000, 47.50000000000000711 ) ) ;
#19555 = DIRECTION ( 'NONE',  ( 1.049727191138617217E-16, 0.5150380749100562650, -0.8571673007021111124 ) ) ;
#19556 = CARTESIAN_POINT ( 'NONE',  ( -13.85640646055084702, -1.500000000000011768, 7.999999999999705125 ) ) ;
#19557 = DIRECTION ( 'NONE',  ( -0.000000000000000000, 1.000000000000000000, -0.000000000000000000 ) ) ;
#19558 = CONICAL_SURFACE ( 'NONE', #8217, 2.099999999999997868, 1.029744258676652091 ) ;
#19559 = CARTESIAN_POINT ( 'NONE',  ( 35.00000000000000000, 22.00000000000000711, -14.99999999999997691 ) ) ;
#19560 = ADVANCED_FACE ( 'NONE', ( #15449 ), #1605, .F. ) ;
#19561 = FACE_BOUND ( 'NONE', #10718, .T. ) ;
#19562 = DIRECTION ( 'NONE',  ( -1.000000000000000000, -1.208970125616062874E-17, 0.000000000000000000 ) ) ;
#19563 = EDGE_CURVE ( 'NONE', #13710, #15616, #13462, .T. ) ;
#19564 = VERTEX_POINT ( 'NONE', #17069 ) ;
#19565 = ORIENTED_EDGE ( 'NONE', *, *, #12979, .F. ) ;
#19566 = EDGE_CURVE ( 'NONE', #14798, #15385, #9137, .T. ) ;
#19567 = ORIENTED_EDGE ( 'NONE', *, *, #16086, .T. ) ;
#19568 = DIRECTION ( 'NONE',  ( 1.296372316667914327E-16, 1.000000000000000000, -0.000000000000000000 ) ) ;
#19569 = CLOSED_SHELL ( 'NONE', ( #21952, #3702, #2603, #16837, #9350, #5821, #8094, #20363, #1891, #7808, #13111, #19124, #7153, #9607, #21196, #11560, #9418, #99, #7696, #8779, #8906, #2311, #6311, #7579, #19560, #20049, #9275, #13432 ) ) ;
#19570 = CARTESIAN_POINT ( 'NONE',  ( 90.00000000000000000, 40.00000000000000711, -9.108981535246192915E-16 ) ) ;
#19571 = AXIS2_PLACEMENT_3D ( 'NONE', #9265, #20157, #21764 ) ;
#19572 = DIRECTION ( 'NONE',  ( -6.505213034913038160E-19, -3.903127820947822896E-18, -1.000000000000000000 ) ) ;
#19573 = FACE_OUTER_BOUND ( 'NONE', #7069, .T. ) ;
#19574 = DIRECTION ( 'NONE',  ( 0.000000000000000000, 1.000000000000000000, 0.000000000000000000 ) ) ;
#19575 = CARTESIAN_POINT ( 'NONE',  ( -12.89955995983995507, 4.696256998628602020, 58.40693116658150785 ) ) ;
#19576 = CARTESIAN_POINT ( 'NONE',  ( -13.73196689449470220, 34.57679379660266505, -56.13071196757329062 ) ) ;
#19577 = DIRECTION ( 'NONE',  ( 1.000000000000000000, 1.208970125616063182E-17, 0.000000000000000000 ) ) ;
#19578 = ORIENTED_EDGE ( 'NONE', *, *, #17917, .F. ) ;
#19579 = FACE_BOUND ( 'NONE', #465, .T. ) ;
#19580 = CARTESIAN_POINT ( 'NONE',  ( -6.775279300855757469, 38.82186504314599773, -55.41168644275258259 ) ) ;
#19581 = PLANE ( 'NONE',  #11884 ) ;
#19582 = CARTESIAN_POINT ( 'NONE',  ( 5.833333333333437842, 6.180730040185884455, -40.61164310337073857 ) ) ;
#19583 = VERTEX_POINT ( 'NONE', #5056 ) ;
#19584 = AXIS2_PLACEMENT_3D ( 'NONE', #11004, #5856, #20170 ) ;
#19585 = CARTESIAN_POINT ( 'NONE',  ( 20.36304159388385671, 24.03323817228478276, 3.000000000000023537 ) ) ;
#19586 = CARTESIAN_POINT ( 'NONE',  ( -15.49999999999980282, -2.516660498395515866, -105.0010000000000048 ) ) ;
#19587 = B_SPLINE_CURVE_WITH_KNOTS ( 'NONE', 3,
 ( #6324, #13068, #6104, #11597 ),
 .UNSPECIFIED., .F., .F.,
 ( 4, 4 ),
 ( 0.001875451646902612842, 0.003761979286330821397 ),
 .UNSPECIFIED. ) ;
#19588 = EDGE_CURVE ( 'NONE', #6416, #16045, #20521, .T. ) ;
#19589 = DIRECTION ( 'NONE',  ( -0.000000000000000000, -0.000000000000000000, 1.000000000000000000 ) ) ;
#19590 = CIRCLE ( 'NONE', #12612, 16.49999999999998579 ) ;
#19591 = ORIENTED_EDGE ( 'NONE', *, *, #22476, .F. ) ;
#19592 = EDGE_CURVE ( 'NONE', #13346, #11018, #3627, .T. ) ;
#19593 = CIRCLE ( 'NONE', #3513, 2.000000000000002665 ) ;
#19594 = VERTEX_POINT ( 'NONE', #10297 ) ;
#19595 = CARTESIAN_POINT ( 'NONE',  ( 0.7921581640248794853, 24.99916066338866116, 8.999720221269573273 ) ) ;
#19596 = AXIS2_PLACEMENT_3D ( 'NONE', #13216, #21616, #6258 ) ;
#19597 = CARTESIAN_POINT ( 'NONE',  ( 35.00000000000000000, 0.000000000000000000, 54.99999999999698019 ) ) ;
#19598 = CARTESIAN_POINT ( 'NONE',  ( 11.85401191286916678, 32.83234229683709771, -2.999999999999995559 ) ) ;
#19599 = VERTEX_POINT ( 'NONE', #20106 ) ;
#19600 = PLANE ( 'NONE',  #22445 ) ;
#19601 = CARTESIAN_POINT ( 'NONE',  ( -8.657949774411953570, 40.00000000000000711, 53.21471414886531193 ) ) ;
#19602 = ORIENTED_EDGE ( 'NONE', *, *, #17783, .F. ) ;
#19603 = FACE_OUTER_BOUND ( 'NONE', #13733, .T. ) ;
#19604 = VECTOR ( 'NONE', #2452, 1000.000000000000000 ) ;
#19605 = CARTESIAN_POINT ( 'NONE',  ( -28.13960001536965194, 21.69517388068233998, -2.999999999999999112 ) ) ;
#19606 = CARTESIAN_POINT ( 'NONE',  ( 15.92429324705532245, 4.173694850190156735, -56.88791232810482512 ) ) ;
#19607 = AXIS2_PLACEMENT_3D ( 'NONE', #16356, #6278, #6389 ) ;
#19608 = DIRECTION ( 'NONE',  ( 0.000000000000000000, 0.000000000000000000, 1.000000000000000000 ) ) ;
#19609 = VERTEX_POINT ( 'NONE', #4826 ) ;
#19610 = CARTESIAN_POINT ( 'NONE',  ( 3.330669073875469621E-13, -1.110223024625156540E-13, -2.999999999999971578 ) ) ;
#19611 = CARTESIAN_POINT ( 'NONE',  ( -1.619914140209613773, 39.98468592336024585, -49.95346900270995150 ) ) ;
#19612 = ORIENTED_EDGE ( 'NONE', *, *, #5686, .T. ) ;
#19613 = CARTESIAN_POINT ( 'NONE',  ( 12.27586057105636108, 4.193657236093890184, 55.54740530680977884 ) ) ;
#19614 = EDGE_CURVE ( 'NONE', #4794, #16628, #18796, .T. ) ;
#19615 = CARTESIAN_POINT ( 'NONE',  ( 1.942890293094023946E-13, -8.326672684688674053E-14, 4.999999999999993783 ) ) ;
#19616 = DIRECTION ( 'NONE',  ( 6.505213034913038160E-19, 3.903127820947822896E-18, 1.000000000000000000 ) ) ;
#19617 = AXIS2_PLACEMENT_3D ( 'NONE', #13746, #19047, #3241 ) ;
#19618 = AXIS2_PLACEMENT_3D ( 'NONE', #2820, #9804, #16795 ) ;
#19619 = CIRCLE ( 'NONE', #16702, 3.000000000000000888 ) ;
#19620 = ORIENTED_EDGE ( 'NONE', *, *, #19614, .T. ) ;
#19621 = VECTOR ( 'NONE', #11669, 1000.000000000000000 ) ;
#19622 = ORIENTED_EDGE ( 'NONE', *, *, #16317, .T. ) ;
#19623 = EDGE_LOOP ( 'NONE', ( #5028, #3428, #7023, #7660 ) ) ;
#19624 =( LENGTH_UNIT ( ) NAMED_UNIT ( * ) SI_UNIT ( .MILLI., .METRE. ) );
#19625 = ORIENTED_EDGE ( 'NONE', *, *, #15805, .T. ) ;
#19626 = DIRECTION ( 'NONE',  ( 0.000000000000000000, 0.000000000000000000, -1.000000000000000000 ) ) ;
#19627 = CARTESIAN_POINT ( 'NONE',  ( -3.469446951953614189E-14, -1.000000000000028644, 48.73397172404114031 ) ) ;
#19628 = CARTESIAN_POINT ( 'NONE',  ( 5.233858753929546914, 39.99999999999999289, -51.72875402900091757 ) ) ;
#19629 = CARTESIAN_POINT ( 'NONE',  ( 6.286720829167179225, 40.00000000000000711, 52.22859680466056176 ) ) ;
#19630 = ORIENTED_EDGE ( 'NONE', *, *, #4579, .F. ) ;
#19631 = DIRECTION ( 'NONE',  ( -1.000000000000000000, -1.208970125616081209E-17, 0.000000000000000000 ) ) ;
#19632 = DIRECTION ( 'NONE',  ( 0.000000000000000000, 0.000000000000000000, -1.000000000000000000 ) ) ;
#19633 = EDGE_LOOP ( 'NONE', ( #13312, #19186, #7128, #12306 ) ) ;
#19634 = AXIS2_PLACEMENT_3D ( 'NONE', #16872, #20540, #1170 ) ;
#19635 = AXIS2_PLACEMENT_3D ( 'NONE', #3550, #2264, #7538 ) ;
#19636 = DIRECTION ( 'NONE',  ( -0.000000000000000000, -1.000000000000000000, -0.000000000000000000 ) ) ;
#19637 = AXIS2_PLACEMENT_3D ( 'NONE', #18482, #2795, #9777 ) ;
#19638 = EDGE_CURVE ( 'NONE', #22194, #3413, #17289, .T. ) ;
#19639 = CARTESIAN_POINT ( 'NONE',  ( -22.42346072916788557, 20.15694599340442394, -58.66711769948890520 ) ) ;
#19640 = AXIS2_PLACEMENT_3D ( 'NONE', #6052, #18310, #18198 ) ;
#19641 = CARTESIAN_POINT ( 'NONE',  ( 36.54278193890331039, 4.025500340002458266, 2.800654218530485018 ) ) ;
#19642 = ORIENTED_EDGE ( 'NONE', *, *, #11663, .T. ) ;
#19643 = B_SPLINE_CURVE_WITH_KNOTS ( 'NONE', 3,
 ( #12130, #22347, #8358, #10285 ),
 .UNSPECIFIED., .F., .F.,
 ( 4, 4 ),
 ( 9.715086409868104685E-07, 0.001929643240672413622 ),
 .UNSPECIFIED. ) ;
#19644 = CARTESIAN_POINT ( 'NONE',  ( 0.6844983420862013057, -1.267142481716289959, 48.72692999687993876 ) ) ;
#19645 = ORIENTED_EDGE ( 'NONE', *, *, #16055, .T. ) ;
#19646 = CARTESIAN_POINT ( 'NONE',  ( 42.50000000000000000, 10.00000000000000000, 49.99999999999999289 ) ) ;
#19647 = DIRECTION ( 'NONE',  ( -1.000000000000000000, -1.208970125616044077E-17, 0.000000000000000000 ) ) ;
#19648 = CARTESIAN_POINT ( 'NONE',  ( -15.62726112422577174, -28.45046755804897387, -6.999999999999971578 ) ) ;
#19649 = EDGE_CURVE ( 'NONE', #1729, #8443, #13727, .T. ) ;
#19650 = EDGE_LOOP ( 'NONE', ( #15379, #18256, #5974, #21283 ) ) ;
#19651 = LINE ( 'NONE', #11038, #2468 ) ;
#19652 = CARTESIAN_POINT ( 'NONE',  ( 18.88991738967228429, 26.58741517403858268, 57.84428223557716819 ) ) ;
#19653 = DIRECTION ( 'NONE',  ( 3.525918314278899701E-15, 0.000000000000000000, 1.000000000000000000 ) ) ;
#19654 = CARTESIAN_POINT ( 'NONE',  ( 13.10473755708325250, 38.28578281281944129, -55.88243319222879535 ) ) ;
#19655 = CIRCLE ( 'NONE', #3186, 6.499999999999999112 ) ;
#19656 = VERTEX_POINT ( 'NONE', #20746 ) ;
#19657 = ORIENTED_EDGE ( 'NONE', *, *, #2636, .F. ) ;
#19658 = EDGE_CURVE ( 'NONE', #15814, #9340, #20810, .T. ) ;
#19659 = ORIENTED_EDGE ( 'NONE', *, *, #9372, .F. ) ;
#19660 = VERTEX_POINT ( 'NONE', #9668 ) ;
#19661 = CARTESIAN_POINT ( 'NONE',  ( -35.00000000000000000, 40.00000000000000000, 1.387778780781445676E-14 ) ) ;
#19662 = VECTOR ( 'NONE', #13867, 999.9999999999998863 ) ;
#19663 = DIRECTION ( 'NONE',  ( 6.505213034913038160E-19, 3.903127820947822896E-18, 1.000000000000000000 ) ) ;
#19664 = DIRECTION ( 'NONE',  ( 0.000000000000000000, 0.000000000000000000, 1.000000000000000000 ) ) ;
#19665 = EDGE_LOOP ( 'NONE', ( #472, #6264, #3018, #6485, #22341 ) ) ;
#19666 = CARTESIAN_POINT ( 'NONE',  ( -12.24744603029288292, 40.00000000000000000, -54.43639671998465701 ) ) ;
#19667 = FACE_OUTER_BOUND ( 'NONE', #20994, .T. ) ;
#19668 = ADVANCED_FACE ( 'NONE', ( #16954 ), #8255, .T. ) ;
#19669 = EDGE_LOOP ( 'NONE', ( #10320, #4302, #22164, #14865 ) ) ;
#19670 = CARTESIAN_POINT ( 'NONE',  ( 16.66666666666666430, -20.00000000000000000, 23.57022603955159212 ) ) ;
#19671 = AXIS2_PLACEMENT_3D ( 'NONE', #261, #14685, #9093 ) ;
#19672 = PRODUCT_DEFINITION_CONTEXT ( 'detailed design', #6086, 'design' ) ;
#19673 = LINE ( 'NONE', #12434, #289 ) ;
#19674 = CARTESIAN_POINT ( 'NONE',  ( 4.177897941877333210, -34.13396246814587442, -6.999999999999950262 ) ) ;
#19675 = CIRCLE ( 'NONE', #9785, 19.11328065563151668 ) ;
#19676 =( LENGTH_UNIT ( ) NAMED_UNIT ( * ) SI_UNIT ( .MILLI., .METRE. ) );
#19677 = CARTESIAN_POINT ( 'NONE',  ( -19.99999999999998934, -4.500000000000007994, 3.306546357697853339E-15 ) ) ;
#19678 = CARTESIAN_POINT ( 'NONE',  ( -42.49999999999996447, 10.00000000000000000, -47.50000000000000711 ) ) ;
#19679 = AXIS2_PLACEMENT_3D ( 'NONE', #8506, #12169, #16882 ) ;
#19680 = CIRCLE ( 'NONE', #17836, 10.00000000000000000 ) ;
#19681 = CARTESIAN_POINT ( 'NONE',  ( 2.775557561562891351E-13, 3.000000000000002665, -5.000000000000004441 ) ) ;
#19682 = VERTEX_POINT ( 'NONE', #12589 ) ;
#19683 = CIRCLE ( 'NONE', #15998, 1.000000000000000888 ) ;
#19684 = ORIENTED_EDGE ( 'NONE', *, *, #11468, .F. ) ;
#19685 = ADVANCED_FACE ( 'NONE', ( #2728 ), #455, .T. ) ;
#19686 = B_SPLINE_CURVE_WITH_KNOTS ( 'NONE', 3,
 ( #18652, #6846, #2959, #10147, #4898, #8552, #5133, #1459, #8669, #8219, #15181, #4790, #8332, #5015, #6499, #20373, #10035, #13465, #3409, #11995, #17366, #1339, #11761, #15305, #8445, #1687, #15648, #22430, #20484, #22328, #15526, #18995, #3183, #20588, #11874, #3302, #18758, #6612, #13574, #17143, #6726, #17254, #5562, #21697, #3526, #8789, #2018, #6962, #5994 ),
 .UNSPECIFIED., .F., .F.,
 ( 4, 1, 1, 1, 2, 2, 1, 1, 1, 1, 2, 2, 1, 1, 1, 2, 2, 1, 1, 1, 1, 2, 2, 1, 1, 1, 1, 2, 2, 1, 1, 1, 2, 2, 4 ),
 ( 0.000000000000000000, 0.1249999999999849842, 0.1874999999999770184, 0.2187499999999730216, 0.2343749999999715228, 0.2499999999999700240, 0.3749999999999616973, 0.4374999999999579781, 0.4687499999999561462, 0.4843749999999556466, 0.4921874999999552580, 0.4999999999999549249, 0.5624999999999592548, 0.5937499999999615863, 0.6093749999999631406, 0.6171874999999638067, 0.6249999999999645839, 0.6874999999999683586, 0.7187499999999701350, 0.7343749999999714673, 0.7421874999999721334, 0.7460937499999724665, 0.7499999999999726885, 0.8124999999999790168, 0.8437499999999827915, 0.8593749999999849010, 0.8671874999999857891, 0.8710937499999861222, 0.8749999999999865663, 0.9062499999999896749, 0.9218749999999912292, 0.9296874999999918954, 0.9335937499999925615, 0.9374999999999932276, 1.000000000000000000 ),
 .UNSPECIFIED. ) ;
#19687 = CIRCLE ( 'NONE', #21139, 1.000000000000000888 ) ;
#19688 = AXIS2_PLACEMENT_3D ( 'NONE', #2864, #17049, #8130 ) ;
#19689 = ORIENTED_EDGE ( 'NONE', *, *, #14942, .T. ) ;
#19690 = FACE_OUTER_BOUND ( 'NONE', #3847, .T. ) ;
#19691 = FACE_OUTER_BOUND ( 'NONE', #21061, .T. ) ;
#19692 = CARTESIAN_POINT ( 'NONE',  ( -35.43359966464135624, 7.197698565811587734, 2.932460736555813963 ) ) ;
#19693 = EDGE_CURVE ( 'NONE', #11286, #5560, #21538, .T. ) ;
#19694 = EDGE_CURVE ( 'NONE', #20280, #12118, #4677, .T. ) ;
#19695 = DIRECTION ( 'NONE',  ( 0.000000000000000000, 0.000000000000000000, -1.000000000000000000 ) ) ;
#19696 =( BOUNDED_SURFACE ( )  B_SPLINE_SURFACE ( 3, 2, ( 
 ( #15766, #20839, #10379 ),
 ( #5357, #12114, #10494 ),
 ( #17496, #19111, #3416 ),
 ( #76, #7064, #14030 ),
 ( #21053, #12334, #19344 ),
 ( #3651, #20131, #3986 ),
 ( #6150, #21732, #6033 ),
 ( #16218, #10955, #16458 ),
 ( #17948, #14831, #13118 ),
 ( #5808, #4436, #4206 ),
 ( #9235, #14613, #16565 ),
 ( #11409, #14718, #5688 ),
 ( #21854, #869, #11065 ),
 ( #21504, #12779, #7862 ) ),
 .UNSPECIFIED., .F., .F., .T. ) 
 B_SPLINE_SURFACE_WITH_KNOTS ( ( 4, 2, 2, 2, 2, 2, 4 ),
 ( 3, 3 ),
 ( 0.004259382447192460938, 0.005809352080732368973, 0.007359321714272276140, 0.008909291347812183307, 0.01045926098135209134, 0.01355920024843190741, 0.01665913951551172348 ),
 ( 0.1636470045611256030, 1.000000000000000000 ),
 .UNSPECIFIED. ) 
 GEOMETRIC_REPRESENTATION_ITEM ( )  RATIONAL_B_SPLINE_SURFACE ( (
 ( 0.9022249821884000820, 0.7012624274003163016, 1.000000000000000000),
 ( 0.9123788763119136114, 0.7322861975901361342, 1.000000000000000000),
 ( 0.9211843504036706376, 0.7591900633693231537, 1.000000000000000000),
 ( 0.9369236066439512456, 0.8072791080863062074, 1.000000000000000000),
 ( 0.9438541764422034852, 0.8284544721476249096, 1.000000000000000000),
 ( 0.9562659320682393993, 0.8663768149956418974, 1.000000000000000000),
 ( 0.9617548100769197639, 0.8831472961401047872, 1.000000000000000000),
 ( 0.9714485269178145810, 0.9127650605070476431, 1.000000000000000000),
 ( 0.9756421407944039226, 0.9255780474842177918, 1.000000000000000000),
 ( 0.9865759213550759910, 0.9589846490593422201, 1.000000000000000000),
 ( 0.9916869380071704487, 0.9746006289112230103, 1.000000000000000000),
 ( 0.9984050399869064396, 0.9951268279631179103, 1.000000000000000000),
 ( 0.9999940432348444208, 0.9999817999566460447, 1.000000000000000000),
 ( 1.000000000000000000, 1.000000000000000000, 1.000000000000000000) ) ) 
 REPRESENTATION_ITEM ( '' )  SURFACE ( )  );
#19697 = CIRCLE ( 'NONE', #9811, 19.11328065563150957 ) ;
#19698 = LINE ( 'NONE', #10849, #22426 ) ;
#19699 = CARTESIAN_POINT ( 'NONE',  ( -13.83098800442514253, 37.66187182509482057, -56.14292165594078909 ) ) ;
#19700 = AXIS2_PLACEMENT_3D ( 'NONE', #4980, #22405, #1773 ) ;
#19701 = AXIS2_PLACEMENT_3D ( 'NONE', #18439, #20608, #10509 ) ;
#19702 = ORIENTED_EDGE ( 'NONE', *, *, #13343, .F. ) ;
#19703 = CARTESIAN_POINT ( 'NONE',  ( -19.05255888325766023, 10.99999999999970512, -5.000000000000004441 ) ) ;
#19704 = VECTOR ( 'NONE', #7401, 1000.000000000000000 ) ;
#19705 = EDGE_CURVE ( 'NONE', #10027, #249, #16142, .T. ) ;
#19706 = CYLINDRICAL_SURFACE ( 'NONE', #17922, 19.11328065563152023 ) ;
#19707 = CARTESIAN_POINT ( 'NONE',  ( 5.999999999999999112, 0.000000000000000000, -6.000000000000000000 ) ) ;
#19708 = LINE ( 'NONE', #14287, #16224 ) ;
#19709 = VECTOR ( 'NONE', #1903, 1000.000000000000114 ) ;
#19710 = ORIENTED_EDGE ( 'NONE', *, *, #9879, .T. ) ;
#19711 = DIRECTION ( 'NONE',  ( -0.9659258262890678681, 0.2588190451025220717, 0.000000000000000000 ) ) ;
#19712 = ORIENTED_EDGE ( 'NONE', *, *, #19026, .F. ) ;
#19713 = DIRECTION ( 'NONE',  ( 1.000000000000000000, 0.000000000000000000, 0.000000000000000000 ) ) ;
#19714 = CARTESIAN_POINT ( 'NONE',  ( 25.99999999999998579, 19.99999999999999645, 100.0000000000000000 ) ) ;
#19715 = CARTESIAN_POINT ( 'NONE',  ( 12.27586057105635042, 4.193657236093891960, -55.54740530680976462 ) ) ;
#19716 = APPLICATION_CONTEXT ( 'automotive_design' ) ;
#19717 = VERTEX_POINT ( 'NONE', #11424 ) ;
#19718 = CONICAL_SURFACE ( 'NONE', #7640, 9.000000000000035527, 0.7853981633974447263 ) ;
#19719 = LINE ( 'NONE', #2283, #9301 ) ;
#19720 = AXIS2_PLACEMENT_3D ( 'NONE', #9099, #17916, #18140 ) ;
#19721 = CIRCLE ( 'NONE', #15675, 49.99999999999998579 ) ;
#19722 = ORIENTED_EDGE ( 'NONE', *, *, #19972, .T. ) ;
#19723 = CARTESIAN_POINT ( 'NONE',  ( 2.670518050928090137, 23.57199239071502817, 8.613211112165400252 ) ) ;
#19724 = CARTESIAN_POINT ( 'NONE',  ( -28.45046755804882110, 15.62726112422596714, 2.999999999999995559 ) ) ;
#19725 = CARTESIAN_POINT ( 'NONE',  ( 35.00000000000000000, -5.000000000000000888, 18.00000000000000711 ) ) ;
#19726 = EDGE_LOOP ( 'NONE', ( #19748, #22042, #1659, #13799 ) ) ;
#19727 = DIRECTION ( 'NONE',  ( -0.000000000000000000, -1.000000000000000000, -0.000000000000000000 ) ) ;
#19728 = LINE ( 'NONE', #2291, #2492 ) ;
#19729 = ORIENTED_EDGE ( 'NONE', *, *, #9477, .T. ) ;
#19730 = CARTESIAN_POINT ( 'NONE',  ( -21.94328778841581595, -28.73472116836736134, 2.932969818539080009 ) ) ;
#19731 = CYLINDRICAL_SURFACE ( 'NONE', #6875, 5.000000000000000000 ) ;
#19732 = EDGE_CURVE ( 'NONE', #790, #9501, #3260, .T. ) ;
#19733 = LINE ( 'NONE', #14425, #7516 ) ;
#19734 = ADVANCED_FACE ( 'NONE', ( #8000 ), #20255, .F. ) ;
#19735 = CARTESIAN_POINT ( 'NONE',  ( 5.833333333333328596, 33.81926995981416439, -40.61164310337066041 ) ) ;
#19736 = ORIENTED_EDGE ( 'NONE', *, *, #19922, .T. ) ;
#19737 = DIRECTION ( 'NONE',  ( -1.000000000000000000, -1.208970125616081209E-17, 0.000000000000000000 ) ) ;
#19738 = CARTESIAN_POINT ( 'NONE',  ( -0.6841746959065087008, -36.75746821813308429, -2.800654218530457484 ) ) ;
#19739 = CIRCLE ( 'NONE', #5817, 2.525000000000110489 ) ;
#19740 = DIRECTION ( 'NONE',  ( 0.1421319796954322312, 0.000000000000000000, 0.9898477157360405787 ) ) ;
#19741 = VERTEX_POINT ( 'NONE', #6383 ) ;
#19742 = EDGE_CURVE ( 'NONE', #18060, #20633, #13347, .T. ) ;
#19743 = DIRECTION ( 'NONE',  ( -0.000000000000000000, 1.000000000000000000, -0.000000000000000000 ) ) ;
#19744 = VERTEX_POINT ( 'NONE', #12821 ) ;
#19745 = ORIENTED_EDGE ( 'NONE', *, *, #16684, .T. ) ;
#19746 = VECTOR ( 'NONE', #20488, 1000.000000000000000 ) ;
#19747 = VERTEX_POINT ( 'NONE', #2293 ) ;
#19748 = ORIENTED_EDGE ( 'NONE', *, *, #22592, .F. ) ;
#19749 = DIRECTION ( 'NONE',  ( 0.000000000000000000, -0.000000000000000000, 1.000000000000000000 ) ) ;
#19750 = CARTESIAN_POINT ( 'NONE',  ( 2.602085213965210642E-15, 6.000000000000019540, 17.00000000000000355 ) ) ;
#19751 = CARTESIAN_POINT ( 'NONE',  ( 7.471708243917213110, 39.63177981526567351, -53.58785989103921565 ) ) ;
#19752 = DIRECTION ( 'NONE',  ( -1.000000000000000000, 0.000000000000000000, 0.000000000000000000 ) ) ;
#19753 = VERTEX_POINT ( 'NONE', #18408 ) ;
#19754 = CARTESIAN_POINT ( 'NONE',  ( -24.99999999999999645, -20.00000000000000000, 16.50000000000000355 ) ) ;
#19755 = LINE ( 'NONE', #18251, #3955 ) ;
#19756 = VERTEX_POINT ( 'NONE', #2185 ) ;
#19757 = CARTESIAN_POINT ( 'NONE',  ( 0.05268221300119596551, -1.234065601521194377, 48.20433757654415530 ) ) ;
#19758 = CYLINDRICAL_SURFACE ( 'NONE', #20699, 3.000000000000002665 ) ;
#19759 = VERTEX_POINT ( 'NONE', #15069 ) ;
#19760 = CARTESIAN_POINT ( 'NONE',  ( 2.775557561562891351E-14, -2.775557561562891351E-14, 2.999999999999999112 ) ) ;
#19761 = EDGE_LOOP ( 'NONE', ( #12868, #18672, #2315, #7576 ) ) ;
#19762 = CARTESIAN_POINT ( 'NONE',  ( 5.340789179572191792, 39.27722415257183286, 54.28402915905950010 ) ) ;
#19763 = CARTESIAN_POINT ( 'NONE',  ( -14.93538271375398274, -34.13396246814581758, 3.000000000000023537 ) ) ;
#19764 = CARTESIAN_POINT ( 'NONE',  ( 15.12081897056669000, -33.51030287062373247, -2.800654218530457484 ) ) ;
#19765 = ORIENTED_EDGE ( 'NONE', *, *, #20258, .F. ) ;
#19766 = AXIS2_PLACEMENT_3D ( 'NONE', #7299, #21165, #5569 ) ;
#19767 = CARTESIAN_POINT ( 'NONE',  ( 19.61594976190319528, 16.00511159616338830, 58.04523854797174920 ) ) ;
#19768 = DIRECTION ( 'NONE',  ( 6.505213034913038160E-19, 3.903127820947822896E-18, 1.000000000000000000 ) ) ;
#19769 = DIRECTION ( 'NONE',  ( 0.000000000000000000, -1.000000000000000000, 0.000000000000000000 ) ) ;
#19771 = ORIENTED_EDGE ( 'NONE', *, *, #7017, .F. ) ;
#19770 = EDGE_CURVE ( 'NONE', #17346, #3823, #9929, .T. ) ;
#19772 = AXIS2_PLACEMENT_3D ( 'NONE', #15577, #9972, #6896 ) ;
#19773 = VERTEX_POINT ( 'NONE', #14307 ) ;
#19774 = ORIENTED_EDGE ( 'NONE', *, *, #4440, .T. ) ;
#19775 = ORIENTED_EDGE ( 'NONE', *, *, #904, .F. ) ;
#19776 = DIRECTION ( 'NONE',  ( 0.000000000000000000, 0.000000000000000000, -1.000000000000000000 ) ) ;
#19777 = CARTESIAN_POINT ( 'NONE',  ( -9.689843208404459673, 39.33333333333334991, -54.54983754392748807 ) ) ;
#19778 = ADVANCED_FACE ( 'NONE', ( #9707 ), #2958, .F. ) ;
#19779 = PLANE ( 'NONE',  #21997 ) ;
#19780 = CIRCLE ( 'NONE', #17575, 16.49999999999998579 ) ;
#19781 = VERTEX_POINT ( 'NONE', #1000 ) ;
#19782 = CARTESIAN_POINT ( 'NONE',  ( 7.474202570536131240, -30.60042966911724704, -2.999999999999999112 ) ) ;
#19783 = CARTESIAN_POINT ( 'NONE',  ( -1.583519045123022995, -4.618580011808621322, 46.65783332780200254 ) ) ;
#19784 = VERTEX_POINT ( 'NONE', #21983 ) ;
#19785 = CARTESIAN_POINT ( 'NONE',  ( 3.399999999999995470, 15.00000000000000178, 0.000000000000000000 ) ) ;
#19786 = LINE ( 'NONE', #13112, #1028 ) ;
#19787 = DIRECTION ( 'NONE',  ( 0.000000000000000000, 1.000000000000000000, 0.000000000000000000 ) ) ;
#19788 = PRESENTATION_STYLE_ASSIGNMENT (( #14493 ) ) ;
#19789 = EDGE_CURVE ( 'NONE', #15811, #19434, #16781, .T. ) ;
#19790 = LINE ( 'NONE', #3864, #3668 ) ;
#19791 = LINE ( 'NONE', #18176, #126 ) ;
#19792 = CARTESIAN_POINT ( 'NONE',  ( 22.98755168577434915, 22.97438720605740770, 2.999999999999999112 ) ) ;
#19793 = ADVANCED_FACE ( 'NONE', ( #19603 ), #13232, .F. ) ;
#19794 = ORIENTED_EDGE ( 'NONE', *, *, #12786, .T. ) ;
#19795 = ORIENTED_EDGE ( 'NONE', *, *, #16315, .T. ) ;
#19796 = AXIS2_PLACEMENT_3D ( 'NONE', #5318, #19188, #8967 ) ;
#19797 = EDGE_LOOP ( 'NONE', ( #11185, #4526, #5666, #14317 ) ) ;
#19798 = ADVANCED_FACE ( 'NONE', ( #3913 ), #13830, .T. ) ;
#19799 = FACE_OUTER_BOUND ( 'NONE', #3196, .T. ) ;
#19800 = VECTOR ( 'NONE', #10566, 1000.000000000000000 ) ;
#19801 = DIRECTION ( 'NONE',  ( 1.000000000000000000, 0.000000000000000000, 0.000000000000000000 ) ) ;
#19802 = CARTESIAN_POINT ( 'NONE',  ( 3.711307361476188671, -1.139702956418044089, -50.71376883234283639 ) ) ;
#19803 = CARTESIAN_POINT ( 'NONE',  ( 0.3107847162787464868, 39.99819769545531756, 49.10452103004165281 ) ) ;
#19804 = DIRECTION ( 'NONE',  ( 6.505213034913038160E-19, 3.903127820947822896E-18, 1.000000000000000000 ) ) ;
#19805 = CARTESIAN_POINT ( 'NONE',  ( 8.479740367036404436, -4.901256658985633230, 50.57596245086651265 ) ) ;
#19806 = CARTESIAN_POINT ( 'NONE',  ( 24.62019382530525391, -4.341204441673157888, -5.000000000000004441 ) ) ;
#19807 = CARTESIAN_POINT ( 'NONE',  ( 14.30873905802343415, 28.06260833510301822, -2.999999999999971578 ) ) ;
#19808 = EDGE_CURVE ( 'NONE', #18161, #1737, #2613, .T. ) ;
#19809 = ORIENTED_EDGE ( 'NONE', *, *, #20783, .F. ) ;
#19810 = DIRECTION ( 'NONE',  ( 0.000000000000000000, 0.000000000000000000, 1.000000000000000000 ) ) ;
#19811 = DIRECTION ( 'NONE',  ( 0.000000000000000000, 0.000000000000000000, 1.000000000000000000 ) ) ;
#19812 = DIRECTION ( 'NONE',  ( 1.000000000000000000, 0.000000000000000000, 0.000000000000000000 ) ) ;
#19813 = CARTESIAN_POINT ( 'NONE',  ( -22.22891329980515707, 23.65408649739117308, -2.999999999999992450 ) ) ;
#19814 = DIRECTION ( 'NONE',  ( 0.000000000000000000, 0.000000000000000000, 1.000000000000000000 ) ) ;
#19815 = VERTEX_POINT ( 'NONE', #5736 ) ;
#19816 = CARTESIAN_POINT ( 'NONE',  ( -33.99999999999998579, 8.251288694035750382, 0.000000000000000000 ) ) ;
#19817 = CYLINDRICAL_SURFACE ( 'NONE', #16275, 19.11328065563152379 ) ;
#19818 = DIRECTION ( 'NONE',  ( 0.000000000000000000, 0.000000000000000000, 1.000000000000000000 ) ) ;
#19819 = ADVANCED_FACE ( 'NONE', ( #6725, #5132 ), #15180, .T. ) ;
#19820 = VERTEX_POINT ( 'NONE', #5236 ) ;
#19821 = CARTESIAN_POINT ( 'NONE',  ( 23.49999999999998579, 19.99999999999999645, 100.0000000000000000 ) ) ;
#19822 = AXIS2_PLACEMENT_3D ( 'NONE', #20634, #20870, #10303 ) ;
#19823 = EDGE_CURVE ( 'NONE', #15170, #4760, #9421, .T. ) ;
#19824 = FACE_OUTER_BOUND ( 'NONE', #5506, .T. ) ;
#19825 = ORIENTED_EDGE ( 'NONE', *, *, #16566, .T. ) ;
#19826 = CARTESIAN_POINT ( 'NONE',  ( 4.592961669381029566, 39.86863535336818387, -51.95971364930980485 ) ) ;
#19827 = CARTESIAN_POINT ( 'NONE',  ( 35.79662727779894738, -4.171001175319904775, -7.000000000000006217 ) ) ;
#19828 = DIRECTION ( 'NONE',  ( -0.000000000000000000, 1.000000000000000000, -0.000000000000000000 ) ) ;
#19829 = ORIENTED_EDGE ( 'NONE', *, *, #13148, .T. ) ;
#19830 = PLANE ( 'NONE',  #4358 ) ;
#19831 = EDGE_CURVE ( 'NONE', #19175, #15847, #16044, .T. ) ;
#19832 = CARTESIAN_POINT ( 'NONE',  ( -9.952189117650803496, 40.00000000000000000, 53.64426396172073908 ) ) ;
#19833 = VERTEX_POINT ( 'NONE', #6961 ) ;
#19834 = CARTESIAN_POINT ( 'NONE',  ( -31.11077005834410159, 4.936596639065010450, -6.999999999999978684 ) ) ;
#19835 = LINE ( 'NONE', #2069, #9448 ) ;
#19836 = CARTESIAN_POINT ( 'NONE',  ( -7.763906758555455312, 40.00000000000000711, 52.86922912568341104 ) ) ;
#19837 = LINE ( 'NONE', #11006, #11508 ) ;
#19838 = EDGE_CURVE ( 'NONE', #21010, #14794, #17507, .T. ) ;
#19839 = EDGE_LOOP ( 'NONE', ( #7751, #19625, #20244, #6135 ) ) ;
#19840 = CARTESIAN_POINT ( 'NONE',  ( 10.27431133777207961, -4.928932188134511172, 51.43682631505490832 ) ) ;
#19841 = CARTESIAN_POINT ( 'NONE',  ( -5.249999999999978684, 40.00000000000000000, 41.42387596543811412 ) ) ;
#19842 = CARTESIAN_POINT ( 'NONE',  ( -6.877234595577741416, 39.69228527894571812, -53.28061377157573020 ) ) ;
#19843 = ORIENTED_EDGE ( 'NONE', *, *, #18562, .T. ) ;
#19844 = DIRECTION ( 'NONE',  ( -1.000000000000000000, 0.000000000000000000, 0.000000000000000000 ) ) ;
#19845 = AXIS2_PLACEMENT_3D ( 'NONE', #9066, #14661, #14196 ) ;
#19846 = DIRECTION ( 'NONE',  ( 0.000000000000000000, 0.000000000000000000, -1.000000000000000000 ) ) ;
#19848 = EDGE_CURVE ( 'NONE', #2199, #22225, #9824, .T. ) ;
#19847 = ORIENTED_EDGE ( 'NONE', *, *, #9831, .F. ) ;
#19849 = ORIENTED_EDGE ( 'NONE', *, *, #13301, .F. ) ;
#19850 = ORIENTED_EDGE ( 'NONE', *, *, #16145, .F. ) ;
#19851 = DIRECTION ( 'NONE',  ( -0.09323006973621358884, -0.9956421404414081966, -0.002209586891662452136 ) ) ;
#19852 = ORIENTED_EDGE ( 'NONE', *, *, #5467, .F. ) ;
#19853 = DIRECTION ( 'NONE',  ( 6.505213034913038160E-19, 3.903127820947822896E-18, 1.000000000000000000 ) ) ;
#19854 = CYLINDRICAL_SURFACE ( 'NONE', #14885, 2.499999999999995115 ) ;
#19855 = AXIS2_PLACEMENT_3D ( 'NONE', #5260, #10284, #22346 ) ;
#19856 = DIRECTION ( 'NONE',  ( 6.505213034913038160E-19, 3.903127820947822896E-18, 1.000000000000000000 ) ) ;
#19857 = LINE ( 'NONE', #16168, #12794 ) ;
#19858 = CARTESIAN_POINT ( 'NONE',  ( -20.00000000000001421, 20.00000000000000000, -60.62177826491068799 ) ) ;
#19859 = ORIENTED_EDGE ( 'NONE', *, *, #10237, .T. ) ;
#19860 = CARTESIAN_POINT ( 'NONE',  ( 7.474202570536158774, -30.60042966911724704, -7.000000000000006217 ) ) ;
#19861 = CARTESIAN_POINT ( 'NONE',  ( 0.000000000000000000, -25.00000000000000000, 19.99999999999999645 ) ) ;
#19862 = ORIENTED_EDGE ( 'NONE', *, *, #8149, .T. ) ;
#19863 = LINE ( 'NONE', #12619, #18925 ) ;
#19864 = CARTESIAN_POINT ( 'NONE',  ( 3.608224830031758756E-13, -2.775557561562891351E-14, -4.999999999999997335 ) ) ;
#19865 = CARTESIAN_POINT ( 'NONE',  ( -21.00948735876881202, -24.79619811426206510, -2.999999999999995559 ) ) ;
#19866 = ORIENTED_EDGE ( 'NONE', *, *, #10020, .T. ) ;
#19867 = CARTESIAN_POINT ( 'NONE',  ( 3.711307361474756927, -1.139702956417446567, 50.71376883234223953 ) ) ;
#19868 = EDGE_LOOP ( 'NONE', ( #3632, #9730, #20041, #20160 ) ) ;
#19869 = CARTESIAN_POINT ( 'NONE',  ( 8.234867195337331580, 38.24532286050943952, 54.56733378486904229 ) ) ;
#19870 = DIRECTION ( 'NONE',  ( -1.000000000000000000, 0.000000000000000000, 0.000000000000000000 ) ) ;
#19871 = VERTEX_POINT ( 'NONE', #8551 ) ;
#19872 = CARTESIAN_POINT ( 'NONE',  ( 21.94328778841601491, 28.73472116836732582, 2.932969818539045814 ) ) ;
#19873 = CYLINDRICAL_SURFACE ( 'NONE', #15822, 2.499999999999998668 ) ;
#19874 = FACE_BOUND ( 'NONE', #284, .T. ) ;
#19876 = ADVANCED_FACE ( 'NONE', ( #6845 ), #4897, .F. ) ;
#19875 = EDGE_LOOP ( 'NONE', ( #8778, #14850, #10876, #17679, #3349, #9465 ) ) ;
#19877 = ORIENTED_EDGE ( 'NONE', *, *, #20384, .T. ) ;
#19878 = ORIENTED_EDGE ( 'NONE', *, *, #18092, .F. ) ;
#19879 = VERTEX_POINT ( 'NONE', #11994 ) ;
#19880 = CARTESIAN_POINT ( 'NONE',  ( 4.104665049622683526, -35.91964150878182238, -2.933296326616347205 ) ) ;
#19881 = CARTESIAN_POINT ( 'NONE',  ( -10.87562399016030135, 39.15903841217814829, -54.97094722855624127 ) ) ;
#19882 = ADVANCED_FACE ( 'NONE', ( #3182 ), #8218, .T. ) ;
#19883 = VERTEX_POINT ( 'NONE', #18994 ) ;
#19884 = CYLINDRICAL_SURFACE ( 'NONE', #5085, 3.999999999999997335 ) ;
#19885 = DIRECTION ( 'NONE',  ( -6.505213034913038160E-19, -3.903127820947822896E-18, -1.000000000000000000 ) ) ;
#19886 = CONICAL_SURFACE ( 'NONE', #18785, 2.099999999999990763, 1.029744258676652091 ) ;
#19887 = EDGE_LOOP ( 'NONE', ( #7618, #9098, #11015, #11892 ) ) ;
#19888 = CARTESIAN_POINT ( 'NONE',  ( 11.86180952234342278, 38.99999999999291589, -55.35904751185374550 ) ) ;
#19889 = DIRECTION ( 'NONE',  ( 0.000000000000000000, 1.000000000000000000, 0.000000000000000000 ) ) ;
#19890 = DIRECTION ( 'NONE',  ( 1.049727191138617217E-16, 0.5150380749100562650, -0.8571673007021111124 ) ) ;
#19891 = DIRECTION ( 'NONE',  ( -0.000000000000000000, -1.000000000000000000, -0.000000000000000000 ) ) ;
#19892 = CIRCLE ( 'NONE', #15104, 2.099999999999997868 ) ;
#19893 = EDGE_CURVE ( 'NONE', #5375, #4097, #11651, .T. ) ;
#19894 = CARTESIAN_POINT ( 'NONE',  ( -29.36548507648019424, -13.83143812983114707, -2.999999999999995559 ) ) ;
#19895 = EDGE_CURVE ( 'NONE', #19583, #11055, #12737, .T. ) ;
#19896 = CIRCLE ( 'NONE', #5623, 15.00000000000000000 ) ;
#19897 = FACE_OUTER_BOUND ( 'NONE', #13121, .T. ) ;
#19898 = CARTESIAN_POINT ( 'NONE',  ( -35.00000000000000000, 7.000000000000000000, -40.99999999999997868 ) ) ;
#19899 = VERTEX_POINT ( 'NONE', #18757 ) ;
#19900 = CIRCLE ( 'NONE', #10363, 2.500000000000002220 ) ;
#19901 = EDGE_LOOP ( 'NONE', ( #14211, #12829, #14151, #10383 ) ) ;
#19902 = CIRCLE ( 'NONE', #6006, 34.90673715956759082 ) ;
#19903 = TOROIDAL_SURFACE ( 'NONE', #130, 50.00000000000000000, 10.00000000000000000 ) ;
#19904 = ORIENTED_EDGE ( 'NONE', *, *, #17441, .F. ) ;
#19905 = LINE ( 'NONE', #4332, #17343 ) ;
#19906 = DIRECTION ( 'NONE',  ( 0.000000000000000000, -1.000000000000000000, 0.000000000000000000 ) ) ;
#19907 = CARTESIAN_POINT ( 'NONE',  ( 1.801771875245271604, 0.06844342149321584745, -51.82845797840088409 ) ) ;
#19908 = LINE ( 'NONE', #11075, #18158 ) ;
#19909 = CARTESIAN_POINT ( 'NONE',  ( 6.401904815323814724, 38.95163572918602313, 55.13655742298573870 ) ) ;
#19910 = LINE ( 'NONE', #10240, #2144 ) ;
#19911 = CARTESIAN_POINT ( 'NONE',  ( -7.555723902514296597, 38.52224445567478028, -55.93227658743224850 ) ) ;
#19912 = DIRECTION ( 'NONE',  ( -6.505213034913038160E-19, -3.903127820947822896E-18, -1.000000000000000000 ) ) ;
#19913 = CYLINDRICAL_SURFACE ( 'NONE', #10200, 6.499999999999999112 ) ;
#19914 = FACE_OUTER_BOUND ( 'NONE', #1188, .T. ) ;
#19915 = PRODUCT_DEFINITION_SHAPE ( 'NONE', 'NONE',  #22706 ) ;
#19916 = CIRCLE ( 'NONE', #7466, 3.999999999999998224 ) ;
#19917 = ORIENTED_EDGE ( 'NONE', *, *, #18017, .F. ) ;
#19918 = DIRECTION ( 'NONE',  ( -1.000000000000000000, 1.775147869274630931E-14, 0.000000000000000000 ) ) ;
#19919 = CARTESIAN_POINT ( 'NONE',  ( -5.302825731643218354, 39.28770244913256704, -54.25167596405762538 ) ) ;
#19920 = CYLINDRICAL_SURFACE ( 'NONE', #19640, 1.000000000000000888 ) ;
#19921 = CARTESIAN_POINT ( 'NONE',  ( 24.75236754129181449, 27.84804035626023477, 2.999999999999995559 ) ) ;
#19922 = EDGE_CURVE ( 'NONE', #12985, #8659, #20587, .T. ) ;
#19923 = ORIENTED_EDGE ( 'NONE', *, *, #14736, .F. ) ;
#19924 = CARTESIAN_POINT ( 'NONE',  ( 12.99999999999993960, 42.51666049839543149, 60.00099999999999767 ) ) ;
#19925 = CARTESIAN_POINT ( 'NONE',  ( -17.32050807568833051, -25.00000000000000000, -10.00000000000047251 ) ) ;
#19926 = DIRECTION ( 'NONE',  ( 0.000000000000000000, 0.000000000000000000, 1.000000000000000000 ) ) ;
#19927 = CIRCLE ( 'NONE', #19204, 25.00000000000000711 ) ;
#19928 = ORIENTED_EDGE ( 'NONE', *, *, #69, .T. ) ;
#19929 = AXIS2_PLACEMENT_3D ( 'NONE', #1351, #11438, #11554 ) ;
#19930 = FACE_OUTER_BOUND ( 'NONE', #18890, .T. ) ;
#19931 = EDGE_CURVE ( 'NONE', #17625, #15936, #111, .T. ) ;
#19932 = DIRECTION ( 'NONE',  ( -1.000000000000000000, -1.208970125616048853E-17, 0.000000000000000000 ) ) ;
#19933 = ORIENTED_EDGE ( 'NONE', *, *, #15340, .F. ) ;
#19934 = CARTESIAN_POINT ( 'NONE',  ( 1.529876220499305495, 39.98623341753695115, -49.88757757837743867 ) ) ;
#19935 = CARTESIAN_POINT ( 'NONE',  ( 35.00000000000001421, 5.000000000000000000, 1.540743955509788682E-30 ) ) ;
#19936 = VERTEX_POINT ( 'NONE', #13687 ) ;
#19937 = DIRECTION ( 'NONE',  ( 1.296372316667914327E-16, 1.000000000000000000, -0.000000000000000000 ) ) ;
#19938 = FACE_OUTER_BOUND ( 'NONE', #2846, .T. ) ;
#19939 = ORIENTED_EDGE ( 'NONE', *, *, #17291, .F. ) ;
#19940 = EDGE_CURVE ( 'NONE', #728, #16668, #10034, .T. ) ;
#19941 = DIRECTION ( 'NONE',  ( 6.505213034913038160E-19, 3.903127820947822896E-18, 1.000000000000000000 ) ) ;
#19942 = CARTESIAN_POINT ( 'NONE',  ( -4.407759405548853593, 40.00000000000000711, 51.31071847168679767 ) ) ;
#19943 = DIRECTION ( 'NONE',  ( -0.000000000000000000, -1.000000000000000000, -0.000000000000000000 ) ) ;
#19944 = ORIENTED_EDGE ( 'NONE', *, *, #11917, .T. ) ;
#19945 = DIRECTION ( 'NONE',  ( -1.000000000000000000, 0.000000000000000000, 0.000000000000000000 ) ) ;
#19946 = AXIS2_PLACEMENT_3D ( 'NONE', #18663, #22217, #10272 ) ;
#19947 = CARTESIAN_POINT ( 'NONE',  ( -11.00126833636917034, 3.276569432483635413, 57.62199738645403357 ) ) ;
#19948 = CARTESIAN_POINT ( 'NONE',  ( -22.15900668633755188, -29.33526866242114295, -2.800654218530433059 ) ) ;
#19949 = TOROIDAL_SURFACE ( 'NONE', #7875, 18.00000000000000711, 0.9999999999999985567 ) ;
#19950 = ORIENTED_EDGE ( 'NONE', *, *, #7114, .F. ) ;
#19951 = CARTESIAN_POINT ( 'NONE',  ( 2.854018578421813982E-15, -6.180736333215565814, 0.000000000000000000 ) ) ;
#19952 = FACE_OUTER_BOUND ( 'NONE', #20923, .T. ) ;
#19953 = CARTESIAN_POINT ( 'NONE',  ( -34.99999999999997868, -5.000000000000000000, 57.49999999999699440 ) ) ;
#19954 = VERTEX_POINT ( 'NONE', #17028 ) ;
#19955 = AXIS2_PLACEMENT_3D ( 'NONE', #15676, #8811, #5263 ) ;
#19956 = ORIENTED_EDGE ( 'NONE', *, *, #9336, .F. ) ;
#19957 = ADVANCED_FACE ( 'NONE', ( #17253 ), #9109, .F. ) ;
#19958 = B_SPLINE_CURVE_WITH_KNOTS ( 'NONE', 3,
 ( #14841, #6043, #12790, #5928, #19909, #6276, #8112, #20256, #11190, #1001, #2729, #13009, #8001, #14960, #21984, #19803, #4215, #18188 ),
 .UNSPECIFIED., .F., .F.,
 ( 4, 2, 2, 2, 2, 2, 2, 2, 4 ),
 ( 0.000000000000000000, 0.001465012583164692446, 0.002930025166329384891, 0.004395037749494077120, 0.005860050332658769782, 0.008790075498988142097, 0.01025508808215282695, 0.01098759437373516244, 0.01172010066531749793 ),
 .UNSPECIFIED. ) ;
#19959 = ORIENTED_EDGE ( 'NONE', *, *, #16392, .T. ) ;
#19960 = UNCERTAINTY_MEASURE_WITH_UNIT (LENGTH_MEASURE( 1.000000000000000082E-05 ), #15026, 'distance_accuracy_value', 'NONE');
#19961 = ORIENTED_EDGE ( 'NONE', *, *, #18233, .T. ) ;
#19962 = CARTESIAN_POINT ( 'NONE',  ( 19.62614308895799908, 23.87978888144414924, -60.53224704373669596 ) ) ;
#19963 = AXIS2_PLACEMENT_3D ( 'NONE', #781, #7762, #14845 ) ;
#19964 = DIRECTION ( 'NONE',  ( 0.000000000000000000, 0.000000000000000000, -1.000000000000000000 ) ) ;
#19965 = CARTESIAN_POINT ( 'NONE',  ( 1.734723475976807094E-14, 20.00000000000000000, 70.71067811865476926 ) ) ;
#19966 = CARTESIAN_POINT ( 'NONE',  ( 2.999999999999998668, 15.99999999999999645, 6.485281374238567764 ) ) ;
#19967 = DIRECTION ( 'NONE',  ( -0.000000000000000000, -0.000000000000000000, 1.000000000000000000 ) ) ;
#19968 = ORIENTED_EDGE ( 'NONE', *, *, #5767, .F. ) ;
#19969 = DIRECTION ( 'NONE',  ( -1.000000000000000000, 1.084202172485464991E-16, 0.000000000000000000 ) ) ;
#19970 = CARTESIAN_POINT ( 'NONE',  ( 30.60042966911749573, 7.474202570535909196, -2.999999999999988898 ) ) ;
#19971 = ORIENTED_EDGE ( 'NONE', *, *, #15348, .T. ) ;
#19972 = EDGE_CURVE ( 'NONE', #22660, #8824, #22327, .T. ) ;
#19973 = EDGE_CURVE ( 'NONE', #17133, #12599, #13573, .T. ) ;
#19974 = CARTESIAN_POINT ( 'NONE',  ( -10.38220159744133575, 9.149172668433822153, -43.52345836121335765 ) ) ;
#19975 = EDGE_CURVE ( 'NONE', #17260, #6902, #8731, .T. ) ;
#19976 = CARTESIAN_POINT ( 'NONE',  ( -21.56999872847277544, 13.83083564369840701, -58.47776649573036423 ) ) ;
#19977 = DIRECTION ( 'NONE',  ( 0.000000000000000000, 0.000000000000000000, 1.000000000000000000 ) ) ;
#19978 = ORIENTED_EDGE ( 'NONE', *, *, #14902, .F. ) ;
#19979 = CARTESIAN_POINT ( 'NONE',  ( 35.00000000000058265, 28.00000000000000000, -52.90000000000076597 ) ) ;
#19980 = CARTESIAN_POINT ( 'NONE',  ( 4.664549341139660577, 0.4975632029829551994, 53.81030450292042389 ) ) ;
#19981 = ORIENTED_EDGE ( 'NONE', *, *, #19893, .T. ) ;
#19982 = CARTESIAN_POINT ( 'NONE',  ( 3.981142735421731249, 39.90683062736657405, 51.58240146861697184 ) ) ;
#19983 = CIRCLE ( 'NONE', #18503, 0.9999999999999974465 ) ;
#19984 = DIRECTION ( 'NONE',  ( -0.000000000000000000, -1.000000000000000000, -0.000000000000000000 ) ) ;
#19985 = CARTESIAN_POINT ( 'NONE',  ( -42.50000000000000711, -5.000000000000000000, 45.40000000000001279 ) ) ;
#19986 = AXIS2_PLACEMENT_3D ( 'NONE', #11850, #22182, #15160 ) ;
#19987 = AXIS2_PLACEMENT_3D ( 'NONE', #11744, #15283, #18738 ) ;
#19988 = ORIENTED_EDGE ( 'NONE', *, *, #16752, .F. ) ;
#19989 = CARTESIAN_POINT ( 'NONE',  ( 11.57708680448565097, 39.19108614651868550, 55.24531487870351754 ) ) ;
#19990 = EDGE_CURVE ( 'NONE', #17804, #20782, #10825, .T. ) ;
#19991 = CARTESIAN_POINT ( 'NONE',  ( -31.21605069118063724, -8.646032897229371628, -2.999999999999971578 ) ) ;
#19992 = CIRCLE ( 'NONE', #15215, 2.499999999999998668 ) ;
#19993 = DIRECTION ( 'NONE',  ( -0.8171172023792284689, 0.3308262969263051634, -0.4720947350246256224 ) ) ;
#19994 = VERTEX_POINT ( 'NONE', #8888 ) ;
#19995 = ORIENTED_EDGE ( 'NONE', *, *, #8147, .T. ) ;
#19996 = ORIENTED_EDGE ( 'NONE', *, *, #7240, .T. ) ;
#19997 = AXIS2_PLACEMENT_3D ( 'NONE', #7311, #17732, #5822 ) ;
#19998 = CONICAL_SURFACE ( 'NONE', #3547, 57.00000000000002132, 0.7853981633974437271 ) ;
#19999 = ORIENTED_EDGE ( 'NONE', *, *, #9014, .T. ) ;
#20000 = CARTESIAN_POINT ( 'NONE',  ( -42.50000000000000711, -5.000000000000000000, -47.50000000000000000 ) ) ;
#20001 = DIRECTION ( 'NONE',  ( -1.000000000000000000, 0.000000000000000000, 0.000000000000000000 ) ) ;
#20002 = AXIS2_PLACEMENT_3D ( 'NONE', #2458, #15442, #15102 ) ;
#20003 = VERTEX_POINT ( 'NONE', #2136 ) ;
#20004 = CYLINDRICAL_SURFACE ( 'NONE', #1047, 1.000000000000000888 ) ;
#20005 = FACE_OUTER_BOUND ( 'NONE', #16971, .T. ) ;
#20006 = ORIENTED_EDGE ( 'NONE', *, *, #16812, .F. ) ;
#20007 = AXIS2_PLACEMENT_3D ( 'NONE', #19347, #12442, #3654 ) ;
#20008 = EDGE_LOOP ( 'NONE', ( #5668, #4232 ) ) ;
#20009 = CYLINDRICAL_SURFACE ( 'NONE', #5705, 36.76383501243555685 ) ;
#20010 = CARTESIAN_POINT ( 'NONE',  ( 3.469446951953614189E-15, 38.23275711891355400, 0.000000000000000000 ) ) ;
#20011 = CARTESIAN_POINT ( 'NONE',  ( 35.00000000000000000, 40.00000000000000000, 4.258610482196280173E-15 ) ) ;
#20012 = EDGE_CURVE ( 'NONE', #18491, #16319, #20085, .T. ) ;
#20013 = ADVANCED_FACE ( 'NONE', ( #7292 ), #12432, .F. ) ;
#20014 = DIRECTION ( 'NONE',  ( -0.000000000000000000, -0.000000000000000000, 1.000000000000000000 ) ) ;
#20015 = VECTOR ( 'NONE', #21782, 1000.000000000000000 ) ;
#20016 = DIRECTION ( 'NONE',  ( -1.000000000000000000, -1.208970125616046080E-17, 6.505213034913038160E-19 ) ) ;
#20017 = DIRECTION ( 'NONE',  ( 0.000000000000000000, 0.000000000000000000, -1.000000000000000000 ) ) ;
#20018 = EDGE_CURVE ( 'NONE', #21174, #15060, #935, .T. ) ;
#20019 = DIRECTION ( 'NONE',  ( 0.000000000000000000, -0.7071067811865500152, -0.7071067811865451302 ) ) ;
#20020 = ORIENTED_EDGE ( 'NONE', *, *, #12288, .T. ) ;
#20021 = CIRCLE ( 'NONE', #3926, 2.099999999999997868 ) ;
#20022 = ORIENTED_EDGE ( 'NONE', *, *, #7358, .F. ) ;
#20023 = EDGE_LOOP ( 'NONE', ( #11660, #6655 ) ) ;
#20024 = FACE_OUTER_BOUND ( 'NONE', #22507, .T. ) ;
#20025 = VECTOR ( 'NONE', #5075, 1000.000000000000000 ) ;
#20026 = DIRECTION ( 'NONE',  ( 0.000000000000000000, 1.000000000000000000, 0.000000000000000000 ) ) ;
#20027 = CARTESIAN_POINT ( 'NONE',  ( 0.3709469612218444512, -0.009390992346624811235, -50.78654667931662914 ) ) ;
#20028 = AXIS2_PLACEMENT_3D ( 'NONE', #2640, #16717, #13251 ) ;
#20029 = ADVANCED_FACE ( 'NONE', ( #10706 ), #2017, .T. ) ;
#20030 = CARTESIAN_POINT ( 'NONE',  ( 21.05198877411829272, -30.13956425491240410, -2.800654218530457484 ) ) ;
#20031 = CYLINDRICAL_SURFACE ( 'NONE', #21836, 28.00000000000001066 ) ;
#20032 = CARTESIAN_POINT ( 'NONE',  ( 1.110223024625156540E-13, -5.551115123125782702E-14, -6.999999999999950262 ) ) ;
#20033 = CARTESIAN_POINT ( 'NONE',  ( -1.387778780781445518E-14, 20.00000000000000355, -102.0000000000000142 ) ) ;
#20034 = FACE_OUTER_BOUND ( 'NONE', #19868, .T. ) ;
#20035 = DIRECTION ( 'NONE',  ( 1.296372316667914327E-16, 1.000000000000000000, -0.000000000000000000 ) ) ;
#20036 = ORIENTED_EDGE ( 'NONE', *, *, #6189, .F. ) ;
#20037 = DIRECTION ( 'NONE',  ( -1.000000000000000000, -3.376276133282418451E-14, 0.000000000000000000 ) ) ;
#20038 = CARTESIAN_POINT ( 'NONE',  ( -0.3107847162787801265, 39.99819769545531756, -49.10452103004165281 ) ) ;
#20039 = DIRECTION ( 'NONE',  ( -1.000000000000000000, 0.000000000000000000, 1.445602896647339163E-16 ) ) ;
#20040 = CARTESIAN_POINT ( 'NONE',  ( -28.45046755804880689, 15.62726112422596714, -7.000000000000006217 ) ) ;
#20041 = ORIENTED_EDGE ( 'NONE', *, *, #9942, .F. ) ;
#20042 = VECTOR ( 'NONE', #11136, 1000.000000000000000 ) ;
#20043 = DIRECTION ( 'NONE',  ( -0.000000000000000000, -0.000000000000000000, -1.000000000000000000 ) ) ;
#20044 = CYLINDRICAL_SURFACE ( 'NONE', #8949, 10.00000000000000178 ) ;
#20045 = AXIS2_PLACEMENT_3D ( 'NONE', #16355, #18190, #20259 ) ;
#20046 = CARTESIAN_POINT ( 'NONE',  ( -32.83234229683724692, 11.85401191286869427, 3.000000000000002665 ) ) ;
#20047 = VECTOR ( 'NONE', #9489, 1000.000000000000114 ) ;
#20048 = EDGE_LOOP ( 'NONE', ( #12812, #5697, #22228, #7916, #7507, #16710 ) ) ;
#20049 = ADVANCED_FACE ( 'NONE', ( #21495, #17709 ), #5461, .F. ) ;
#20050 = DIRECTION ( 'NONE',  ( -1.224646799147353207E-16, 1.000000000000000000, 0.000000000000000000 ) ) ;
#20051 = CIRCLE ( 'NONE', #9048, 18.42595423422130452 ) ;
#20052 = DIRECTION ( 'NONE',  ( 0.000000000000000000, 0.000000000000000000, -1.000000000000000000 ) ) ;
#20053 = VERTEX_POINT ( 'NONE', #7169 ) ;
#20054 = CARTESIAN_POINT ( 'NONE',  ( 2.673152730111972630, 14.43024452475228614, 8.612623190900158932 ) ) ;
#20055 = EDGE_CURVE ( 'NONE', #12680, #7125, #5680, .T. ) ;
#20056 = AXIS2_PLACEMENT_3D ( 'NONE', #3208, #7082, #15550 ) ;
#20057 = CARTESIAN_POINT ( 'NONE',  ( 32.75570538720779012, -15.02862401740828702, -2.999999999999964473 ) ) ;
#20058 = CIRCLE ( 'NONE', #16015, 2.099999999999997868 ) ;
#20059 = DIRECTION ( 'NONE',  ( 0.000000000000000000, 0.000000000000000000, 1.000000000000000000 ) ) ;
#20060 = CARTESIAN_POINT ( 'NONE',  ( -4.416367413074144821, 40.00000000000001421, 51.31508042366087352 ) ) ;
#20061 = LINE ( 'NONE', #18678, #11240 ) ;
#20062 = DIRECTION ( 'NONE',  ( -6.505213034913038160E-19, -3.903127820947822896E-18, -1.000000000000000000 ) ) ;
#20063 = CARTESIAN_POINT ( 'NONE',  ( 34.99999999999999289, -5.000000000000000000, -52.49999999999705835 ) ) ;
#20064 = ORIENTED_EDGE ( 'NONE', *, *, #2621, .T. ) ;
#20065 = CARTESIAN_POINT ( 'NONE',  ( -42.50000000000000711, -12.00000000000012434, -47.50000000000000000 ) ) ;
#20066 = CARTESIAN_POINT ( 'NONE',  ( -34.99999999999999289, 1.000000000000044187, -3.012171160963566127E-14 ) ) ;
#20067 = CARTESIAN_POINT ( 'NONE',  ( -0.02632564323144977528, 39.99999593179830981, -48.75445554395042080 ) ) ;
#20068 = ORIENTED_EDGE ( 'NONE', *, *, #5597, .T. ) ;
#20069 = ADVANCED_FACE ( 'NONE', ( #9124 ), #16099, .F. ) ;
#20070 = CIRCLE ( 'NONE', #12363, 19.99999999999999289 ) ;
#20071 = DIRECTION ( 'NONE',  ( -1.000000000000000000, 0.000000000000000000, 0.000000000000000000 ) ) ;
#20072 = CARTESIAN_POINT ( 'NONE',  ( -22.22891329980529562, 23.65408649739109137, 2.999999999999995559 ) ) ;
#20073 = AXIS2_PLACEMENT_3D ( 'NONE', #14818, #2932, #16789 ) ;
#20074 = CIRCLE ( 'NONE', #305, 19.00000000000000355 ) ;
#20075 = CONICAL_SURFACE ( 'NONE', #21170, 2.525000000000110489, 0.7853981633971014453 ) ;
#20076 = EDGE_CURVE ( 'NONE', #18701, #8987, #21821, .T. ) ;
#20077 = AXIS2_PLACEMENT_3D ( 'NONE', #3687, #17877, #7219 ) ;
#20078 = VERTEX_POINT ( 'NONE', #21383 ) ;
#20079 = VERTEX_POINT ( 'NONE', #5801 ) ;
#20080 = SHAPE_REPRESENTATION_RELATIONSHIP ( 'NONE' , 'NONE' ,  #10907, #13154 ) ;
#20081 = VERTEX_POINT ( 'NONE', #12654 ) ;
#20082 = CARTESIAN_POINT ( 'NONE',  ( 14.64427171882021028, 33.62973864230776400, -59.05294378005808653 ) ) ;
#20083 = LINE ( 'NONE', #8049, #17216 ) ;
#20084 = CARTESIAN_POINT ( 'NONE',  ( -15.50000000000011013, 42.51666049839536043, -105.0010000000000048 ) ) ;
#20085 = CIRCLE ( 'NONE', #22289, 0.9999999999999974465 ) ;
#20086 = SPHERICAL_SURFACE ( 'NONE', #674, 41.25806096964027603 ) ;
#20087 = ORIENTED_EDGE ( 'NONE', *, *, #20522, .F. ) ;
#20088 = CARTESIAN_POINT ( 'NONE',  ( 6.696867368503558448E-15, 40.00000000000000000, 38.73397172404480671 ) ) ;
#20090 = AXIS2_PLACEMENT_3D ( 'NONE', #17195, #20640, #1509 ) ;
#20089 = DIRECTION ( 'NONE',  ( 6.505213034913038160E-19, 3.903127820947822896E-18, 1.000000000000000000 ) ) ;
#20091 = ORIENTED_EDGE ( 'NONE', *, *, #20750, .F. ) ;
#20092 = CARTESIAN_POINT ( 'NONE',  ( -22.29010897948493763, 17.41268129326156355, -58.63841251601397175 ) ) ;
#20093 = CARTESIAN_POINT ( 'NONE',  ( 0.7785676492820222672, 40.00000000000002842, 49.23936426806961464 ) ) ;
#20094 = VERTEX_POINT ( 'NONE', #19670 ) ;
#20095 = DIRECTION ( 'NONE',  ( 0.000000000000000000, 0.000000000000000000, 1.000000000000000000 ) ) ;
#20096 = DIRECTION ( 'NONE',  ( 0.000000000000000000, 1.000000000000000000, 0.000000000000000000 ) ) ;
#20097 = EDGE_LOOP ( 'NONE', ( #21308, #18906, #22260, #15239 ) ) ;
#20098 = CARTESIAN_POINT ( 'NONE',  ( 1.575018543176820440, 39.98856470501870319, 49.93405373658204383 ) ) ;
#20099 =( GEOMETRIC_REPRESENTATION_CONTEXT ( 3 ) GLOBAL_UNCERTAINTY_ASSIGNED_CONTEXT ( ( #9665 ) ) GLOBAL_UNIT_ASSIGNED_CONTEXT ( ( #9869, #4155, #9532 ) ) REPRESENTATION_CONTEXT ( 'NONE', 'WORKASPACE' ) );
#20100 = CARTESIAN_POINT ( 'NONE',  ( 7.604730156747764556E-14, -1.031417236136237481, -48.34206739765565430 ) ) ;
#20101 = ORIENTED_EDGE ( 'NONE', *, *, #16215, .F. ) ;
#20102 = CARTESIAN_POINT ( 'NONE',  ( -35.00000000000000000, 38.99999999999999289, 1.387778780781445676E-14 ) ) ;
#20103 = EDGE_CURVE ( 'NONE', #19660, #21037, #17777, .T. ) ;
#20104 = LINE ( 'NONE', #13086, #10772 ) ;
#20105 = CYLINDRICAL_SURFACE ( 'NONE', #11444, 18.00000000000000000 ) ;
#20106 = CARTESIAN_POINT ( 'NONE',  ( 35.00000000000000000, -9.000000000000001776, 14.00000000000000355 ) ) ;
#20107 = CARTESIAN_POINT ( 'NONE',  ( 17.37021972826951455, 10.07190481803176318, -57.39172882205954807 ) ) ;
#20108 = ADVANCED_FACE ( 'NONE', ( #10948 ), #16208, .F. ) ;
#20109 = EDGE_LOOP ( 'NONE', ( #204, #14817, #22244, #21795, #20558, #835 ) ) ;
#20110 = EDGE_LOOP ( 'NONE', ( #2592, #2240 ) ) ;
#20111 = ORIENTED_EDGE ( 'NONE', *, *, #12534, .T. ) ;
#20112 = ADVANCED_FACE ( 'NONE', ( #5099 ), #18725, .F. ) ;
#20113 = ORIENTED_EDGE ( 'NONE', *, *, #6511, .T. ) ;
#20114 = CARTESIAN_POINT ( 'NONE',  ( 11.52370268964480005, 39.05614286667413637, 55.22012726439884744 ) ) ;
#20115 = CARTESIAN_POINT ( 'NONE',  ( 42.50000000000000711, -12.00000000000000000, 45.00000000000000711 ) ) ;
#20116 = PRODUCT ( 'SEAL', 'SEAL', '', ( #12146 ) ) ;
#20117 = ADVANCED_FACE ( 'NONE', ( #19335 ), #22559, .F. ) ;
#20118 = ORIENTED_EDGE ( 'NONE', *, *, #3240, .F. ) ;
#20119 = FACE_OUTER_BOUND ( 'NONE', #6771, .T. ) ;
#20120 = ORIENTED_EDGE ( 'NONE', *, *, #5252, .T. ) ;
#20121 = DIRECTION ( 'NONE',  ( 0.000000000000000000, -1.000000000000000000, 0.000000000000000000 ) ) ;
#20122 = AXIS2_PLACEMENT_3D ( 'NONE', #21248, #16731, #14585 ) ;
#20123 = ORIENTED_EDGE ( 'NONE', *, *, #15461, .T. ) ;
#20124 = CARTESIAN_POINT ( 'NONE',  ( 36.75746821813311271, -0.6841746959068695233, -1.999999999999994893 ) ) ;
#20125 = EDGE_CURVE ( 'NONE', #2949, #2277, #14833, .T. ) ;
#20126 = CARTESIAN_POINT ( 'NONE',  ( -20.00000000000001421, 20.00000000000000355, 60.62177826491070931 ) ) ;
#20127 = CARTESIAN_POINT ( 'NONE',  ( -34.88850421923980605, 1.128083539116031542, 2.999999999999995559 ) ) ;
#20128 = DIRECTION ( 'NONE',  ( 0.000000000000000000, 0.000000000000000000, -1.000000000000000000 ) ) ;
#20129 = EDGE_CURVE ( 'NONE', #12073, #943, #21157, .T. ) ;
#20130 = AXIS2_PLACEMENT_3D ( 'NONE', #4943, #11923, #18922 ) ;
#20131 = CARTESIAN_POINT ( 'NONE',  ( -6.297086633636163278, 38.99689310884462401, 53.73982279751612623 ) ) ;
#20132 = CARTESIAN_POINT ( 'NONE',  ( -12.00937115242649256, -34.74700806321106938, -2.800654218530485018 ) ) ;
#20133 = ORIENTED_EDGE ( 'NONE', *, *, #21533, .F. ) ;
#20134 = ORIENTED_EDGE ( 'NONE', *, *, #22364, .F. ) ;
#20135 = CIRCLE ( 'NONE', #1468, 6.499999999999999112 ) ;
#20136 = EDGE_CURVE ( 'NONE', #14267, #12579, #9353, .T. ) ;
#20137 = ORIENTED_EDGE ( 'NONE', *, *, #7839, .F. ) ;
#20138 = CARTESIAN_POINT ( 'NONE',  ( -21.60519577075148590, 26.10363331747822357, 58.48615516158935179 ) ) ;
#20139 = CYLINDRICAL_SURFACE ( 'NONE', #892, 31.50000000000000711 ) ;
#20140 = EDGE_CURVE ( 'NONE', #19936, #6468, #1312, .T. ) ;
#20141 = DIRECTION ( 'NONE',  ( -0.000000000000000000, 1.000000000000000000, -0.000000000000000000 ) ) ;
#20142 = DIRECTION ( 'NONE',  ( 1.296372316667914327E-16, 1.000000000000000000, -0.000000000000000000 ) ) ;
#20143 = APPLICATION_CONTEXT ( 'automotive_design' ) ;
#20144 = CIRCLE ( 'NONE', #1855, 2.000000000000000888 ) ;
#20145 = DIRECTION ( 'NONE',  ( 0.000000000000000000, 0.000000000000000000, 1.000000000000000000 ) ) ;
#20146 = EDGE_CURVE ( 'NONE', #12403, #15891, #14477, .T. ) ;
#20147 = DIRECTION ( 'NONE',  ( 0.000000000000000000, 0.000000000000000000, 1.000000000000000000 ) ) ;
#20148 = CARTESIAN_POINT ( 'NONE',  ( -5.204760841428789142, 39.83793900407623312, -52.32476308507700224 ) ) ;
#20149 = CARTESIAN_POINT ( 'NONE',  ( -35.00000000000000000, 17.00000000000000000, 39.00000000000003553 ) ) ;
#20150 = VERTEX_POINT ( 'NONE', #6361 ) ;
#20151 = DIRECTION ( 'NONE',  ( -1.000000000000000000, -1.208970125616046080E-17, 6.505213034913038160E-19 ) ) ;
#20152 = CARTESIAN_POINT ( 'NONE',  ( 4.171001175319571708, 35.79662727779881237, -6.999999999999950262 ) ) ;
#20153 = CARTESIAN_POINT ( 'NONE',  ( 19.67606655124947324, 9.154757266467395738, 58.01240525280897486 ) ) ;
#20154 = FACE_OUTER_BOUND ( 'NONE', #19247, .T. ) ;
#20155 = EDGE_LOOP ( 'NONE', ( #4517, #7412, #12643, #7671 ) ) ;
#20156 = DIRECTION ( 'NONE',  ( 1.000000000000000000, 0.000000000000000000, 0.000000000000000000 ) ) ;
#20157 = DIRECTION ( 'NONE',  ( -6.505213034913038160E-19, -3.903127820947822896E-18, -1.000000000000000000 ) ) ;
#20158 = CARTESIAN_POINT ( 'NONE',  ( -35.00000000000000000, 39.00000000000000711, 1.387778780781445676E-14 ) ) ;
#20159 = AXIS2_PLACEMENT_3D ( 'NONE', #10905, #19513, #15826 ) ;
#20160 = ORIENTED_EDGE ( 'NONE', *, *, #748, .F. ) ;
#20161 = EDGE_CURVE ( 'NONE', #9888, #4759, #9703, .T. ) ;
#20162 = CARTESIAN_POINT ( 'NONE',  ( 34.99999999999980815, 40.00000000000000000, 54.99999999999922551 ) ) ;
#20163 = CARTESIAN_POINT ( 'NONE',  ( 3.807409362178445278, 39.99999999999999289, -50.99570508274572234 ) ) ;
#20164 = EDGE_LOOP ( 'NONE', ( #15048, #15232, #2088, #16957 ) ) ;
#20165 = CARTESIAN_POINT ( 'NONE',  ( 4.436829441114990225, 39.87775404803028323, -51.86208824299732356 ) ) ;
#20166 = DIRECTION ( 'NONE',  ( 6.505213034913038160E-19, 3.903127820947822896E-18, 1.000000000000000000 ) ) ;
#20167 = CYLINDRICAL_SURFACE ( 'NONE', #16192, 0.9999999999999974465 ) ;
#20168 = CARTESIAN_POINT ( 'NONE',  ( 34.99999999999980815, 26.00000000000000355, 54.99999999999922551 ) ) ;
#20169 = CYLINDRICAL_SURFACE ( 'NONE', #18580, 31.50000000000000711 ) ;
#20170 = DIRECTION ( 'NONE',  ( 1.000000000000000000, 0.000000000000000000, 0.000000000000000000 ) ) ;
#20171 = CIRCLE ( 'NONE', #17235, 3.000000000000002665 ) ;
#20172 = CARTESIAN_POINT ( 'NONE',  ( 35.00000000000000711, 40.00000000000000000, 58.99999999999995026 ) ) ;
#20173 = ORIENTED_EDGE ( 'NONE', *, *, #18123, .T. ) ;
#20174 = CARTESIAN_POINT ( 'NONE',  ( -13.00000000000011546, 42.51666049839536043, -100.0000000000000000 ) ) ;
#20175 = DIRECTION ( 'NONE',  ( 0.000000000000000000, 0.000000000000000000, -1.000000000000000000 ) ) ;
#20176 = CARTESIAN_POINT ( 'NONE',  ( 8.923978417723413159, 2.083761144195372950, -56.51262908347433722 ) ) ;
#20177 = DIRECTION ( 'NONE',  ( 0.000000000000000000, 0.000000000000000000, 1.000000000000000000 ) ) ;
#20178 = ADVANCED_FACE ( 'NONE', ( #6142 ), #6429, .T. ) ;
#20179 = ORIENTED_EDGE ( 'NONE', *, *, #1066, .T. ) ;
#20180 = CARTESIAN_POINT ( 'NONE',  ( -1.387778780781445518E-14, 20.00000000000000355, -100.0000000000000000 ) ) ;
#20181 = DIRECTION ( 'NONE',  ( 6.505213034913038160E-19, 3.903127820947822896E-18, 1.000000000000000000 ) ) ;
#20182 = LINE ( 'NONE', #16623, #4895 ) ;
#20183 = EDGE_CURVE ( 'NONE', #17988, #10690, #4428, .T. ) ;
#20184 = CIRCLE ( 'NONE', #17618, 1.000000000000000888 ) ;
#20185 = VECTOR ( 'NONE', #17535, 1000.000000000000000 ) ;
#20186 = ORIENTED_EDGE ( 'NONE', *, *, #22109, .F. ) ;
#20187 = B_SPLINE_CURVE_WITH_KNOTS ( 'NONE', 3,
 ( #5470, #1915, #21169, #3315 ),
 .UNSPECIFIED., .F., .F.,
 ( 4, 4 ),
 ( 0.001875451646903046523, 0.003761979286331322732 ),
 .UNSPECIFIED. ) ;
#20188 = VERTEX_POINT ( 'NONE', #4657 ) ;
#20189 = DIRECTION ( 'NONE',  ( -0.003596745190944640024, -0.001882447320459650769, 0.9999917598741085989 ) ) ;
#20190 = ORIENTED_EDGE ( 'NONE', *, *, #15222, .F. ) ;
#20191 = CARTESIAN_POINT ( 'NONE',  ( 18.85684496195309023, 26.68267098057082976, 60.33873919100126670 ) ) ;
#20192 = DIRECTION ( 'NONE',  ( 1.000000000000000000, 0.000000000000000000, 0.000000000000000000 ) ) ;
#20193 = CARTESIAN_POINT ( 'NONE',  ( -0.7857880201100420070, 25.00083595504507983, 9.000278651541817609 ) ) ;
#20194 = CARTESIAN_POINT ( 'NONE',  ( -34.99999999999997868, -5.000000000000000000, 54.99999999999698730 ) ) ;
#20195 = FACE_OUTER_BOUND ( 'NONE', #5830, .T. ) ;
#20196 = ORIENTED_EDGE ( 'NONE', *, *, #4764, .T. ) ;
#20197 = DIRECTION ( 'NONE',  ( 0.000000000000000000, 0.000000000000000000, 1.000000000000000000 ) ) ;
#20198 = CARTESIAN_POINT ( 'NONE',  ( 34.09180625983512414, 10.01331137436145013, -2.999999999999984901 ) ) ;
#20199 = VERTEX_POINT ( 'NONE', #18046 ) ;
#20200 = CARTESIAN_POINT ( 'NONE',  ( 0.000000000000000000, 9.999999999999998224, 3.399999999999995026 ) ) ;
#20201 = DIRECTION ( 'NONE',  ( -0.000000000000000000, 1.000000000000000000, -0.000000000000000000 ) ) ;
#20202 = CIRCLE ( 'NONE', #20573, 4.999999999999997335 ) ;
#20203 = DIRECTION ( 'NONE',  ( 0.000000000000000000, 1.000000000000000000, 0.000000000000000000 ) ) ;
#20204 = DIRECTION ( 'NONE',  ( -0.000000000000000000, -0.000000000000000000, -1.000000000000000000 ) ) ;
#20205 = VERTEX_POINT ( 'NONE', #21965 ) ;
#20206 = CARTESIAN_POINT ( 'NONE',  ( -42.50000000000000711, -9.600000000000001421, -50.00000000000000000 ) ) ;
#20207 = FACE_OUTER_BOUND ( 'NONE', #21112, .T. ) ;
#20208 = VERTEX_POINT ( 'NONE', #639 ) ;
#20209 = CARTESIAN_POINT ( 'NONE',  ( 90.00000000000000000, 28.00000000000000000, -9.108981535246192915E-16 ) ) ;
#20210 = EDGE_CURVE ( 'NONE', #10262, #9329, #16673, .T. ) ;
#20211 = CARTESIAN_POINT ( 'NONE',  ( -0.5687583343899257349, -4.666323447581314454, -48.32169744526334654 ) ) ;
#20212 = CARTESIAN_POINT ( 'NONE',  ( -9.103081159019540181, 0.03030367950604016467, 53.87333532811888404 ) ) ;
#20213 = EDGE_LOOP ( 'NONE', ( #10386, #14535 ) ) ;
#20214 = UNCERTAINTY_MEASURE_WITH_UNIT (LENGTH_MEASURE( 1.000000000000000082E-05 ), #17560, 'distance_accuracy_value', 'NONE');
#20215 = DIRECTION ( 'NONE',  ( 1.000000000000000000, 0.000000000000000000, 0.000000000000000000 ) ) ;
#20216 = FACE_OUTER_BOUND ( 'NONE', #5632, .T. ) ;
#20217 = EDGE_CURVE ( 'NONE', #14227, #9695, #7632, .T. ) ;
#20218 = CARTESIAN_POINT ( 'NONE',  ( 22.29474960931338856, 17.42887675327984098, -58.63958600108815489 ) ) ;
#20219 = ORIENTED_EDGE ( 'NONE', *, *, #15246, .T. ) ;
#20220 = CONICAL_SURFACE ( 'NONE', #3392, 15.99999999999993072, 0.7853981633974415066 ) ;
#20221 = ORIENTED_EDGE ( 'NONE', *, *, #2380, .F. ) ;
#20222 = EDGE_LOOP ( 'NONE', ( #20290, #6567, #17899, #16295 ) ) ;
#20223 = ORIENTED_EDGE ( 'NONE', *, *, #7467, .F. ) ;
#20224 = DIRECTION ( 'NONE',  ( 0.000000000000000000, 0.000000000000000000, 1.000000000000000000 ) ) ;
#20225 = DIRECTION ( 'NONE',  ( 0.000000000000000000, 1.000000000000000000, 0.000000000000000000 ) ) ;
#20226 = ADVANCED_FACE ( 'NONE', ( #6255 ), #20009, .T. ) ;
#20227 = VERTEX_POINT ( 'NONE', #20233 ) ;
#20228 = DIRECTION ( 'NONE',  ( 1.000000000000000000, 1.208970125616063182E-17, 0.000000000000000000 ) ) ;
#20229 = CARTESIAN_POINT ( 'NONE',  ( -8.306841138099667177, 0.005341471314548606325, -53.48947974199504074 ) ) ;
#20230 = VERTEX_POINT ( 'NONE', #11523 ) ;
#20231 = FACE_OUTER_BOUND ( 'NONE', #3027, .T. ) ;
#20232 = ORIENTED_EDGE ( 'NONE', *, *, #12103, .T. ) ;
#20233 = CARTESIAN_POINT ( 'NONE',  ( -11.99999999999999289, 12.49999999999999822, 0.000000000000000000 ) ) ;
#20234 = CARTESIAN_POINT ( 'NONE',  ( -34.99999999999999289, 0.000000000000000000, 11.00000000000000888 ) ) ;
#20235 = EDGE_CURVE ( 'NONE', #15368, #19564, #591, .T. ) ;
#20236 = DIRECTION ( 'NONE',  ( 1.000000000000000000, 1.208970125616063182E-17, 0.000000000000000000 ) ) ;
#20237 = EDGE_CURVE ( 'NONE', #14416, #16284, #22067, .T. ) ;
#20238 = CARTESIAN_POINT ( 'NONE',  ( -16.44544766657918444, 31.39195386311722302, -59.65016313815161197 ) ) ;
#20239 = CIRCLE ( 'NONE', #10327, 33.99999999999999289 ) ;
#20240 = VECTOR ( 'NONE', #15843, 1000.000000000000000 ) ;
#20241 = DIRECTION ( 'NONE',  ( -0.000000000000000000, -1.000000000000000000, -0.000000000000000000 ) ) ;
#20242 = LINE ( 'NONE', #18292, #11216 ) ;
#20243 = EDGE_CURVE ( 'NONE', #13151, #2902, #10777, .T. ) ;
#20244 = ORIENTED_EDGE ( 'NONE', *, *, #3317, .T. ) ;
#20245 = EDGE_LOOP ( 'NONE', ( #9788, #9941 ) ) ;
#20246 = ADVANCED_FACE ( 'NONE', ( #2481 ), #20360, .F. ) ;
#20247 = ORIENTED_EDGE ( 'NONE', *, *, #11764, .T. ) ;
#20248 = CARTESIAN_POINT ( 'NONE',  ( -17.37021972826562077, 10.07190481803563742, 57.39172882205629378 ) ) ;
#20249 = CARTESIAN_POINT ( 'NONE',  ( -10.00000000000000888, 3.000000000000002665, 5.000000000000000888 ) ) ;
#20250 = AXIS2_PLACEMENT_3D ( 'NONE', #12532, #21263, #6016 ) ;
#20251 = EDGE_CURVE ( 'NONE', #7580, #15404, #10223, .T. ) ;
#20252 = CARTESIAN_POINT ( 'NONE',  ( -25.00000000000000000, 20.00000000000000000, 6.487780019669002523E-15 ) ) ;
#20253 = CARTESIAN_POINT ( 'NONE',  ( -10.36558328700373011, 39.99999999999999289, 53.76404159467914923 ) ) ;
#20254 = CIRCLE ( 'NONE', #6707, 1.000000000000000888 ) ;
#20255 = CYLINDRICAL_SURFACE ( 'NONE', #21177, 16.49999999999998579 ) ;
#20256 = CARTESIAN_POINT ( 'NONE',  ( 4.589682443554551128, 39.46972628399738170, 53.62209933471819312 ) ) ;
#20257 = CARTESIAN_POINT ( 'NONE',  ( 35.00000000000000000, 0.000000000000000000, -38.99999999999997868 ) ) ;
#20258 = EDGE_CURVE ( 'NONE', #21090, #5871, #21723, .T. ) ;
#20259 = DIRECTION ( 'NONE',  ( 0.000000000000000000, 0.000000000000000000, -1.000000000000000000 ) ) ;
#20260 = EDGE_CURVE ( 'NONE', #14751, #15922, #1435, .T. ) ;
#20261 = LINE ( 'NONE', #18191, #11174 ) ;
#20262 = ADVANCED_FACE ( 'NONE', ( #16901 ), #8422, .T. ) ;
#20263 = ORIENTED_EDGE ( 'NONE', *, *, #7254, .F. ) ;
#20264 = CIRCLE ( 'NONE', #4532, 2.499999999999996891 ) ;
#20265 = CARTESIAN_POINT ( 'NONE',  ( -10.74988822594902693, 39.17840323696252369, 54.92437902628115864 ) ) ;
#20266 = CARTESIAN_POINT ( 'NONE',  ( 11.68090480754629645, 3.765577839755392731, 57.90797000640142045 ) ) ;
#20267 = CARTESIAN_POINT ( 'NONE',  ( -90.00000000000000000, 28.00000000000000000, -2.099999999999991651 ) ) ;
#20268 = EDGE_CURVE ( 'NONE', #7946, #9114, #14089, .T. ) ;
#20269 = VERTEX_POINT ( 'NONE', #13663 ) ;
#20270 = CIRCLE ( 'NONE', #12924, 2.099999999999997868 ) ;
#20271 = FACE_OUTER_BOUND ( 'NONE', #18157, .T. ) ;
#20272 = CARTESIAN_POINT ( 'NONE',  ( 32.40961249803553557, -2.422192751864171711, 2.999999999999995559 ) ) ;
#20273 = CARTESIAN_POINT ( 'NONE',  ( 30.07487443287981677, -12.31876324338301920, -2.999999999999999112 ) ) ;
#20274 = EDGE_CURVE ( 'NONE', #20847, #4626, #10242, .T. ) ;
#20275 = CONICAL_SURFACE ( 'NONE', #1952, 58.99999999999701572, 0.7853981633974447263 ) ;
#20276 = B_SPLINE_CURVE_WITH_KNOTS ( 'NONE', 3,
 ( #15665, #14270, #12343, #8687 ),
 .UNSPECIFIED., .F., .F.,
 ( 4, 4 ),
 ( 0.001875451646903004022, 0.003761979286331056885 ),
 .UNSPECIFIED. ) ;
#20277 = FACE_OUTER_BOUND ( 'NONE', #6674, .T. ) ;
#20278 = AXIS2_PLACEMENT_3D ( 'NONE', #22534, #3626, #3509 ) ;
#20279 = CARTESIAN_POINT ( 'NONE',  ( -14.74639653023204744, 28.96193690644924246, -7.000000000000006217 ) ) ;
#20280 = VERTEX_POINT ( 'NONE', #8529 ) ;
#20281 = CARTESIAN_POINT ( 'NONE',  ( 0.7619088751511168267, 39.99660921569888217, -49.31788807117369799 ) ) ;
#20282 = DIRECTION ( 'NONE',  ( 1.000000000000000000, 0.000000000000000000, 0.000000000000000000 ) ) ;
#20283 = CIRCLE ( 'NONE', #10378, 19.11328065563151668 ) ;
#20284 = DIRECTION ( 'NONE',  ( -6.505213034913038160E-19, -3.903127820947822896E-18, -1.000000000000000000 ) ) ;
#20285 = CARTESIAN_POINT ( 'NONE',  ( 42.49999999999998579, 10.00000000000000000, -47.49999999999997868 ) ) ;
#20286 = LINE ( 'NONE', #11345, #654 ) ;
#20287 = AXIS2_PLACEMENT_3D ( 'NONE', #11687, #18683, #2988 ) ;
#20288 = CARTESIAN_POINT ( 'NONE',  ( 22.28024240313505899, 22.26748298433242468, -7.000000000000006217 ) ) ;
#20289 = CARTESIAN_POINT ( 'NONE',  ( 1.734723475976807094E-14, -20.00000000000000000, -70.71067811865476926 ) ) ;
#20290 = ORIENTED_EDGE ( 'NONE', *, *, #8578, .T. ) ;
#20291 = CARTESIAN_POINT ( 'NONE',  ( 35.16985127952418111, 10.70799354677351367, -2.800654218530464146 ) ) ;
#20292 = CARTESIAN_POINT ( 'NONE',  ( 9.103081159015154356, 0.03030367950454006254, 53.87333532811640424 ) ) ;
#20293 = CARTESIAN_POINT ( 'NONE',  ( 7.505578006075176667, 1.461761173328237851, -55.63523492904085543 ) ) ;
#20294 = DIRECTION ( 'NONE',  ( 0.000000000000000000, -1.000000000000000000, 0.000000000000000000 ) ) ;
#20295 = ADVANCED_FACE ( 'NONE', ( #20464 ), #20679, .F. ) ;
#20296 = ORIENTED_EDGE ( 'NONE', *, *, #6597, .F. ) ;
#20297 = ADVANCED_FACE ( 'NONE', ( #13555, #22306 ), #1662, .T. ) ;
#20298 = AXIS2_PLACEMENT_3D ( 'NONE', #21934, #2791, #13293 ) ;
#20299 = DIRECTION ( 'NONE',  ( 0.000000000000000000, -1.000000000000000000, 0.000000000000000000 ) ) ;
#20300 = CARTESIAN_POINT ( 'NONE',  ( -34.10919265018073077, 11.98978967046168265, 2.932969818539067575 ) ) ;
#20301 = PRODUCT_DEFINITION_SHAPE ( 'NONE', 'NONE',  #22703 ) ;
#20302 = EDGE_CURVE ( 'NONE', #3679, #5453, #16682, .T. ) ;
#20303 = AXIS2_PLACEMENT_3D ( 'NONE', #5831, #11083, #18075 ) ;
#20304 = ORIENTED_EDGE ( 'NONE', *, *, #13669, .T. ) ;
#20305 = ORIENTED_EDGE ( 'NONE', *, *, #21938, .F. ) ;
#20306 = ORIENTED_EDGE ( 'NONE', *, *, #16782, .T. ) ;
#20307 = CARTESIAN_POINT ( 'NONE',  ( 10.45842016914148509, 40.00000000000000000, 53.79442460303516782 ) ) ;
#20308 = CARTESIAN_POINT ( 'NONE',  ( -5.093313992686310243, -32.09841355226006243, 2.999999999999995559 ) ) ;
#20309 = FACE_BOUND ( 'NONE', #18711, .T. ) ;
#20310 = CARTESIAN_POINT ( 'NONE',  ( 34.99999999999999289, 0.000000000000000000, -52.49999999999705835 ) ) ;
#20311 = DIRECTION ( 'NONE',  ( 0.000000000000000000, 0.000000000000000000, 1.000000000000000000 ) ) ;
#20312 = ORIENTED_EDGE ( 'NONE', *, *, #4150, .F. ) ;
#20313 = DIRECTION ( 'NONE',  ( 6.505213034913038160E-19, 3.903127820947822896E-18, 1.000000000000000000 ) ) ;
#20314 = FACE_OUTER_BOUND ( 'NONE', #10924, .T. ) ;
#20315 = ORIENTED_EDGE ( 'NONE', *, *, #18741, .F. ) ;
#20316 = CARTESIAN_POINT ( 'NONE',  ( 21.00948735876911755, 24.79619811426203668, 3.000000000000006217 ) ) ;
#20317 = PLANE ( 'NONE',  #18893 ) ;
#20318 = CONICAL_SURFACE ( 'NONE', #10408, 10.00000000000000000, 0.7853981633974447263 ) ;
#20319 = ADVANCED_FACE ( 'NONE', ( #6478 ), #12642, .F. ) ;
#20320 = LINE ( 'NONE', #16974, #9705 ) ;
#20321 = CARTESIAN_POINT ( 'NONE',  ( 4.406385930812127150, 39.99999999999999289, 51.31001910650969222 ) ) ;
#20322 = ORIENTED_EDGE ( 'NONE', *, *, #18123, .F. ) ;
#20323 = CARTESIAN_POINT ( 'NONE',  ( 0.000000000000000000, 28.49999999999998934, 0.000000000000000000 ) ) ;
#20324 = CARTESIAN_POINT ( 'NONE',  ( 7.928368521050060735, 38.36676511147830126, -56.15748794203490490 ) ) ;
#20325 = ORIENTED_EDGE ( 'NONE', *, *, #10402, .F. ) ;
#20326 = CARTESIAN_POINT ( 'NONE',  ( -42.50000000000000711, -12.00000000000000000, 49.60000000000000853 ) ) ;
#20327 = ORIENTED_EDGE ( 'NONE', *, *, #3705, .F. ) ;
#20328 = CARTESIAN_POINT ( 'NONE',  ( 14.19004819996276723, 37.38003124960520296, 56.27686160268850557 ) ) ;
#20329 = DIRECTION ( 'NONE',  ( -0.000000000000000000, -0.000000000000000000, -1.000000000000000000 ) ) ;
#20330 = CIRCLE ( 'NONE', #13336, 2.500000000000002220 ) ;
#20331 = AXIS2_PLACEMENT_3D ( 'NONE', #19019, #17624, #14049 ) ;
#20332 = CARTESIAN_POINT ( 'NONE',  ( 18.94109686629718681, 13.34133107273948227, -60.36587731981236260 ) ) ;
#20333 = EDGE_LOOP ( 'NONE', ( #9521, #7266, #5863, #6112 ) ) ;
#20334 = CIRCLE ( 'NONE', #14062, 0.9999999999999974465 ) ;
#20335 = ORIENTED_EDGE ( 'NONE', *, *, #7957, .F. ) ;
#20336 = ORIENTED_EDGE ( 'NONE', *, *, #8361, .F. ) ;
#20337 = ADVANCED_FACE ( 'NONE', ( #3043 ), #5037, .F. ) ;
#20338 = ORIENTED_EDGE ( 'NONE', *, *, #5785, .T. ) ;
#20339 = CARTESIAN_POINT ( 'NONE',  ( 27.19760187735889545, 24.73600648735091312, 2.800654218530485018 ) ) ;
#20340 = DIRECTION ( 'NONE',  ( 0.000000000000000000, 0.000000000000000000, 1.000000000000000000 ) ) ;
#20341 = PRODUCT_DEFINITION ( 'UNKNOWN', '', #324, #6234 ) ;
#20342 = ORIENTED_EDGE ( 'NONE', *, *, #19065, .T. ) ;
#20343 = DIRECTION ( 'NONE',  ( -0.000000000000000000, -1.000000000000000000, -0.000000000000000000 ) ) ;
#20344 = CARTESIAN_POINT ( 'NONE',  ( -9.367793990838201523, -4.928932186899944057, -51.00106331755883105 ) ) ;
#20345 = VERTEX_POINT ( 'NONE', #12512 ) ;
#20346 = VECTOR ( 'NONE', #5516, 1000.000000000000000 ) ;
#20347 = CARTESIAN_POINT ( 'NONE',  ( -3.000000000000000000, 15.20121272115292044, 8.485281374238567764 ) ) ;
#20348 = AXIS2_PLACEMENT_3D ( 'NONE', #3280, #10244, #17233 ) ;
#20349 = DIRECTION ( 'NONE',  ( -0.000000000000000000, -1.000000000000000000, -0.000000000000000000 ) ) ;
#20350 = ORIENTED_EDGE ( 'NONE', *, *, #12946, .F. ) ;
#20351 = CARTESIAN_POINT ( 'NONE',  ( -7.577104390338862849, -0.4826542685308932157, -53.01683071947938686 ) ) ;
#20352 = CIRCLE ( 'NONE', #22183, 19.11328065563150957 ) ;
#20353 = CARTESIAN_POINT ( 'NONE',  ( 4.163799117100995136E-16, 9.999999999999998224, -3.399999999999995026 ) ) ;
#20354 = DIRECTION ( 'NONE',  ( 6.505213034913038160E-19, 3.903127820947822896E-18, 1.000000000000000000 ) ) ;
#20355 = CARTESIAN_POINT ( 'NONE',  ( -19.01465036493458882, 26.21927150370769866, -60.37937655616647703 ) ) ;
#20356 = VECTOR ( 'NONE', #13013, 1000.000000000000000 ) ;
#20357 = LINE ( 'NONE', #15398, #20685 ) ;
#20358 = EDGE_CURVE ( 'NONE', #968, #6991, #3535, .T. ) ;
#20359 = AXIS2_PLACEMENT_3D ( 'NONE', #1336, #2838, #8329 ) ;
#20360 = CONICAL_SURFACE ( 'NONE', #10814, 49.99999999999998579, 0.7853981633974657095 ) ;
#20361 = EDGE_LOOP ( 'NONE', ( #2672, #14898, #3129, #17681 ) ) ;
#20362 = VERTEX_POINT ( 'NONE', #1994 ) ;
#20363 = ADVANCED_FACE ( 'NONE', ( #17459 ), #8976, .T. ) ;
#20364 = EDGE_LOOP ( 'NONE', ( #9238, #59 ) ) ;
#20365 = CARTESIAN_POINT ( 'NONE',  ( -14.89439646620539293, 6.624450698086694622, 59.14252023618892906 ) ) ;
#20366 = AXIS2_PLACEMENT_3D ( 'NONE', #4691, #12914, #6288 ) ;
#20367 = DIRECTION ( 'NONE',  ( -6.505213034913038160E-19, -3.903127820947822896E-18, -1.000000000000000000 ) ) ;
#20368 = DIRECTION ( 'NONE',  ( -0.000000000000000000, -1.000000000000000000, -0.000000000000000000 ) ) ;
#20369 = CARTESIAN_POINT ( 'NONE',  ( -28.06260833510287966, 14.30873905802324053, 2.999999999999995559 ) ) ;
#20370 = CARTESIAN_POINT ( 'NONE',  ( -17.99805307122279174, -21.44924440733175786, 3.000000000000023537 ) ) ;
#20371 = ORIENTED_EDGE ( 'NONE', *, *, #14414, .T. ) ;
#20372 = CARTESIAN_POINT ( 'NONE',  ( -31.57187188083528184, -7.711478842616553919, 3.000000000000023537 ) ) ;
#20373 = CARTESIAN_POINT ( 'NONE',  ( -4.794048179926227782, 40.00000000000000000, -51.50619363643422588 ) ) ;
#20374 = CARTESIAN_POINT ( 'NONE',  ( 33.51030287062395274, 15.12081897056660651, 2.800654218530485018 ) ) ;
#20375 = DIRECTION ( 'NONE',  ( 1.000000000000000000, 0.000000000000000000, 0.000000000000000000 ) ) ;
#20376 = FACE_OUTER_BOUND ( 'NONE', #13767, .T. ) ;
#20377 = CIRCLE ( 'NONE', #5000, 0.9999999999999956701 ) ;
#20378 = VERTEX_POINT ( 'NONE', #21246 ) ;
#20379 = LINE ( 'NONE', #3188, #5146 ) ;
#20380 = CYLINDRICAL_SURFACE ( 'NONE', #22527, 2.099999999999997868 ) ;
#20381 = VECTOR ( 'NONE', #18018, 1000.000000000000000 ) ;
#20382 = VERTEX_POINT ( 'NONE', #268 ) ;
#20383 = CARTESIAN_POINT ( 'NONE',  ( 35.00000000000000000, 13.99999999999999822, 2.255140518769849223E-14 ) ) ;
#20384 = EDGE_CURVE ( 'NONE', #1842, #20949, #6066, .T. ) ;
#20385 = FACE_OUTER_BOUND ( 'NONE', #8642, .T. ) ;
#20386 = CARTESIAN_POINT ( 'NONE',  ( -42.50000000000000000, 7.000000000000000000, 47.49999999999999289 ) ) ;
#20387 = ORIENTED_EDGE ( 'NONE', *, *, #10758, .T. ) ;
#20388 = ADVANCED_FACE ( 'NONE', ( #3725 ), #9729, .T. ) ;
#20389 = AXIS2_PLACEMENT_3D ( 'NONE', #9410, #12935, #13162 ) ;
#20390 = EDGE_LOOP ( 'NONE', ( #5959, #22288 ) ) ;
#20391 = CARTESIAN_POINT ( 'NONE',  ( -9.370858128257053110, -4.928932186902839518, 51.00253624878534708 ) ) ;
#20392 = DIRECTION ( 'NONE',  ( -0.000000000000000000, -1.000000000000000000, -0.000000000000000000 ) ) ;
#20393 = ORIENTED_EDGE ( 'NONE', *, *, #12957, .T. ) ;
#20394 = CARTESIAN_POINT ( 'NONE',  ( 14.68506606271058779, 16.91806408329018652, 45.68712064066588141 ) ) ;
#20395 = ADVANCED_FACE ( 'NONE', ( #5652 ), #8992, .T. ) ;
#20396 = CARTESIAN_POINT ( 'NONE',  ( -14.74639653023206165, 28.96193690644924246, -2.999999999999968026 ) ) ;
#20397 = CARTESIAN_POINT ( 'NONE',  ( 7.711478842616581453, -31.57187188083526763, -2.999999999999995559 ) ) ;
#20398 = CARTESIAN_POINT ( 'NONE',  ( 1.110223024625156540E-13, -5.551115123125782702E-14, -6.999999999999950262 ) ) ;
#20399 = CARTESIAN_POINT ( 'NONE',  ( -13.25963002225075371, 27.02330685613478423, -45.02656532858657812 ) ) ;
#20400 = CIRCLE ( 'NONE', #21493, 36.76383501243555685 ) ;
#20401 = DIRECTION ( 'NONE',  ( 0.000000000000000000, 0.000000000000000000, 1.000000000000000000 ) ) ;
#20402 = ORIENTED_EDGE ( 'NONE', *, *, #13168, .T. ) ;
#20403 = CARTESIAN_POINT ( 'NONE',  ( 14.69988787053502222, 23.08500126984896639, 45.69379240540679632 ) ) ;
#20404 = CIRCLE ( 'NONE', #12340, 16.49999999999999645 ) ;
#20405 = CARTESIAN_POINT ( 'NONE',  ( 1.485717122675112911, -1.299971956346694490, 49.29290837556793292 ) ) ;
#20406 = CARTESIAN_POINT ( 'NONE',  ( 7.505578006075174891, 1.461761173328240071, -55.63523492904086254 ) ) ;
#20407 = CARTESIAN_POINT ( 'NONE',  ( -0.1621100730513900801, 39.99984845991361482, -48.85976302750078304 ) ) ;
#20408 = CIRCLE ( 'NONE', #21864, 1.000000000000000888 ) ;
#20409 = VERTEX_POINT ( 'NONE', #14230 ) ;
#20410 = DIRECTION ( 'NONE',  ( -6.505213034913038160E-19, -3.903127820947822896E-18, -1.000000000000000000 ) ) ;
#20411 = DIRECTION ( 'NONE',  ( -1.000000000000000000, -1.208970125616077665E-17, 0.000000000000000000 ) ) ;
#20412 = CIRCLE ( 'NONE', #19322, 60.00000000000000000 ) ;
#20413 = CIRCLE ( 'NONE', #1007, 60.00000000000000000 ) ;
#20414 = ORIENTED_EDGE ( 'NONE', *, *, #320, .F. ) ;
#20415 = CIRCLE ( 'NONE', #17478, 2.500000000000002220 ) ;
#20416 = CIRCLE ( 'NONE', #10516, 5.000000000000000000 ) ;
#20417 = ORIENTED_EDGE ( 'NONE', *, *, #251, .F. ) ;
#20418 = ITEM_DEFINED_TRANSFORMATION ( 'NONE', 'NONE', #14949,  #18273 ) ;
#20419 = EDGE_CURVE ( 'NONE', #13179, #9457, #1693, .T. ) ;
#20420 = ORIENTED_EDGE ( 'NONE', *, *, #19319, .F. ) ;
#20421 = CARTESIAN_POINT ( 'NONE',  ( 9.144347024359401388, 37.80953375799288807, 56.77060857467738941 ) ) ;
#20422 = CARTESIAN_POINT ( 'NONE',  ( 11.68090480754629112, 3.765577839755377187, -57.90797000640139913 ) ) ;
#20423 = CARTESIAN_POINT ( 'NONE',  ( -42.50000000000000711, -12.00000000000012434, -50.02500000000011227 ) ) ;
#20424 = EDGE_CURVE ( 'NONE', #19747, #6187, #5326, .T. ) ;
#20425 = DIRECTION ( 'NONE',  ( -0.000000000000000000, 1.000000000000000000, -0.000000000000000000 ) ) ;
#20426 = CARTESIAN_POINT ( 'NONE',  ( 3.601266574137822474, 5.429865540864382112, -39.39030536259068782 ) ) ;
#20427 = EDGE_LOOP ( 'NONE', ( #18881, #16181, #7338, #20501 ) ) ;
#20428 = DIRECTION ( 'NONE',  ( -0.1421319796954322034, 0.000000000000000000, 0.9898477157360405787 ) ) ;
#20429 = CARTESIAN_POINT ( 'NONE',  ( -8.646032897229066094, 31.21605069118044185, 2.999999999999995559 ) ) ;
#20430 = ORIENTED_EDGE ( 'NONE', *, *, #20217, .F. ) ;
#20431 = CARTESIAN_POINT ( 'NONE',  ( -14.04383866228955746, 14.71638174774082941, -45.39674436955349535 ) ) ;
#20432 = FACE_OUTER_BOUND ( 'NONE', #6103, .T. ) ;
#20433 = PLANE ( 'NONE',  #21049 ) ;
#20434 = CARTESIAN_POINT ( 'NONE',  ( 13.76051559511272693, 5.481080969678164827, -58.73291665846257104 ) ) ;
#20435 = ORIENTED_EDGE ( 'NONE', *, *, #3104, .F. ) ;
#20436 = DIRECTION ( 'NONE',  ( 0.000000000000000000, 0.000000000000000000, 1.000000000000000000 ) ) ;
#20437 = EDGE_CURVE ( 'NONE', #19583, #5633, #2105, .T. ) ;
#20438 = ORIENTED_EDGE ( 'NONE', *, *, #2984, .F. ) ;
#20439 = DIRECTION ( 'NONE',  ( 0.000000000000000000, 0.000000000000000000, -1.000000000000000000 ) ) ;
#20440 = CARTESIAN_POINT ( 'NONE',  ( -0.6847309795004193900, -1.267153214277350948, -48.72709510502366470 ) ) ;
#20441 = CIRCLE ( 'NONE', #6170, 51.00000000000002132 ) ;
#20442 = ORIENTED_EDGE ( 'NONE', *, *, #21685, .F. ) ;
#20443 = PLANE ( 'NONE',  #19679 ) ;
#20444 = AXIS2_PLACEMENT_3D ( 'NONE', #7193, #17733, #5482 ) ;
#20445 = VECTOR ( 'NONE', #14825, 1000.000000000000114 ) ;
#20446 = DIRECTION ( 'NONE',  ( -0.000000000000000000, -1.000000000000000000, -0.000000000000000000 ) ) ;
#20447 = DIRECTION ( 'NONE',  ( -1.000000000000000000, 2.033026488858229532E-14, 0.000000000000000000 ) ) ;
#20448 = CARTESIAN_POINT ( 'NONE',  ( 15.91215689494260843, 32.15331685092851188, -56.91770382337011114 ) ) ;
#20449 = VERTEX_POINT ( 'NONE', #12307 ) ;
#20450 = ORIENTED_EDGE ( 'NONE', *, *, #11335, .F. ) ;
#20451 = AXIS2_PLACEMENT_3D ( 'NONE', #16696, #17883, #14959 ) ;
#20452 = ORIENTED_EDGE ( 'NONE', *, *, #19033, .T. ) ;
#20453 = ORIENTED_EDGE ( 'NONE', *, *, #196, .F. ) ;
#20454 = CARTESIAN_POINT ( 'NONE',  ( -21.41958700883256483, -27.56232195404059837, 2.999999999999995559 ) ) ;
#20455 = AXIS2_PLACEMENT_3D ( 'NONE', #21152, #63, #17704 ) ;
#20456 = FACE_OUTER_BOUND ( 'NONE', #14598, .T. ) ;
#20457 = ORIENTED_EDGE ( 'NONE', *, *, #16309, .F. ) ;
#20458 = CARTESIAN_POINT ( 'NONE',  ( 4.044183821322609990E-15, 3.000000000000006217, 0.000000000000000000 ) ) ;
#20459 = CARTESIAN_POINT ( 'NONE',  ( -0.7837852459083360923, 13.10023700646259037, 6.967910395774163490 ) ) ;
#20460 = VERTEX_POINT ( 'NONE', #9205 ) ;
#20461 = AXIS2_PLACEMENT_3D ( 'NONE', #12262, #19269, #17301 ) ;
#20462 = DIRECTION ( 'NONE',  ( 6.505213034913038160E-19, 3.903127820947822896E-18, 1.000000000000000000 ) ) ;
#20463 = VERTEX_POINT ( 'NONE', #19646 ) ;
#20464 = FACE_OUTER_BOUND ( 'NONE', #4830, .T. ) ;
#20465 = DIRECTION ( 'NONE',  ( -0.000000000000000000, -1.000000000000000000, -0.000000000000000000 ) ) ;
#20466 = CARTESIAN_POINT ( 'NONE',  ( -14.93538271375420479, -34.13396246814581758, -2.999999999999999112 ) ) ;
#20467 = CARTESIAN_POINT ( 'NONE',  ( -18.31820558117436448, 28.04217374067966873, -60.19578215372065699 ) ) ;
#20468 = AXIS2_PLACEMENT_3D ( 'NONE', #17791, #2096, #14335 ) ;
#20469 = EDGE_CURVE ( 'NONE', #15106, #12184, #16251, .T. ) ;
#20470 = CARTESIAN_POINT ( 'NONE',  ( -13.08927703801865405, 12.63446361230554693, 44.94509734929668809 ) ) ;
#20471 =( GEOMETRIC_REPRESENTATION_CONTEXT ( 3 ) GLOBAL_UNCERTAINTY_ASSIGNED_CONTEXT ( ( #18368 ) ) GLOBAL_UNIT_ASSIGNED_CONTEXT ( ( #1763, #13544, #15266 ) ) REPRESENTATION_CONTEXT ( 'NONE', 'WORKASPACE' ) );
#20472 = ORIENTED_EDGE ( 'NONE', *, *, #17772, .T. ) ;
#20473 = EDGE_CURVE ( 'NONE', #573, #2168, #21837, .T. ) ;
#20474 = ORIENTED_EDGE ( 'NONE', *, *, #8027, .F. ) ;
#20475 = ORIENTED_EDGE ( 'NONE', *, *, #5332, .T. ) ;
#20476 = CARTESIAN_POINT ( 'NONE',  ( -18.94109686629600731, 13.34133107273681595, 60.36587731981239813 ) ) ;
#20477 = DIRECTION ( 'NONE',  ( 0.000000000000000000, -1.000000000000000000, 0.000000000000000000 ) ) ;
#20478 = AXIS2_PLACEMENT_3D ( 'NONE', #329, #7320, #14285 ) ;
#20479 = DIRECTION ( 'NONE',  ( 0.000000000000000000, 0.000000000000000000, 1.000000000000000000 ) ) ;
#20480 = CARTESIAN_POINT ( 'NONE',  ( -14.74639653023204744, 28.96193690644924246, -7.000000000000006217 ) ) ;
#20481 = CYLINDRICAL_SURFACE ( 'NONE', #10813, 31.50000000000001421 ) ;
#20482 = ORIENTED_EDGE ( 'NONE', *, *, #14922, .T. ) ;
#20483 = DIRECTION ( 'NONE',  ( -1.000000000000000000, 0.000000000000000000, 0.000000000000000000 ) ) ;
#20484 = CARTESIAN_POINT ( 'NONE',  ( -7.287850675723428040, 40.00000000000000000, -52.67053208787582719 ) ) ;
#20485 = CARTESIAN_POINT ( 'NONE',  ( -23.50000000000001066, 19.99999999999982947, 60.00099999999999767 ) ) ;
#20486 = CARTESIAN_POINT ( 'NONE',  ( 42.50000000000000711, -9.600000000000001421, -47.50000000000000000 ) ) ;
#20487 = ORIENTED_EDGE ( 'NONE', *, *, #103, .F. ) ;
#20488 = DIRECTION ( 'NONE',  ( 0.000000000000000000, 0.000000000000000000, -1.000000000000000000 ) ) ;
#20489 = ADVANCED_FACE ( 'NONE', ( #10578 ), #1825, .F. ) ;
#20490 = ORIENTED_EDGE ( 'NONE', *, *, #3834, .T. ) ;
#20491 = DIRECTION ( 'NONE',  ( -6.505213034913038160E-19, -3.903127820947822896E-18, -1.000000000000000000 ) ) ;
#20492 = VECTOR ( 'NONE', #2487, 1000.000000000000000 ) ;
#20493 = CARTESIAN_POINT ( 'NONE',  ( 1.734723475976807094E-14, 20.00000000000000000, 70.71067811865476926 ) ) ;
#20494 = DIRECTION ( 'NONE',  ( 0.000000000000000000, 0.000000000000000000, 1.000000000000000000 ) ) ;
#20495 = ORIENTED_EDGE ( 'NONE', *, *, #19742, .T. ) ;
#20496 = EDGE_CURVE ( 'NONE', #18353, #13383, #11378, .T. ) ;
#20497 = ORIENTED_EDGE ( 'NONE', *, *, #18707, .T. ) ;
#20498 = CARTESIAN_POINT ( 'NONE',  ( -5.095494235770363645, -3.097009620008996045, 50.75850000587684718 ) ) ;
#20499 = CIRCLE ( 'NONE', #17584, 17.00000000000000355 ) ;
#20500 = CARTESIAN_POINT ( 'NONE',  ( 12.99999999999993960, 42.51666049839543149, -105.0010000000000048 ) ) ;
#20501 = ORIENTED_EDGE ( 'NONE', *, *, #18064, .F. ) ;
#20502 = CARTESIAN_POINT ( 'NONE',  ( 10.63866000424707003, 9.419394561690063838, 43.66469350997158472 ) ) ;
#20503 = EDGE_CURVE ( 'NONE', #14743, #15720, #6455, .T. ) ;
#20504 = AXIS2_PLACEMENT_3D ( 'NONE', #2558, #16521, #19752 ) ;
#20505 = DIRECTION ( 'NONE',  ( -0.000000000000000000, -1.000000000000000000, -0.000000000000000000 ) ) ;
#20506 = CARTESIAN_POINT ( 'NONE',  ( -5.074925817841608122, 32.10132595304110481, 3.000000000000016431 ) ) ;
#20507 = CARTESIAN_POINT ( 'NONE',  ( -19.61594976190323081, 16.00511159616170431, -58.04523854797172078 ) ) ;
#20508 = CARTESIAN_POINT ( 'NONE',  ( 25.99999999999998579, 19.99999999999999645, 60.00099999999999767 ) ) ;
#20509 = CARTESIAN_POINT ( 'NONE',  ( -15.91215689494263330, 32.15331685092852609, 56.91770382337013245 ) ) ;
#20510 = VERTEX_POINT ( 'NONE', #9660 ) ;
#20511 = DIRECTION ( 'NONE',  ( 1.000000000000000000, 0.000000000000000000, 0.000000000000000000 ) ) ;
#20512 = SURFACE_STYLE_FILL_AREA ( #12029 ) ;
#20513 = CARTESIAN_POINT ( 'NONE',  ( 9.867969867548763929, 0.2954100743914914728, -54.30456930252559289 ) ) ;
#20514 = EDGE_CURVE ( 'NONE', #6211, #2785, #22191, .T. ) ;
#20515 = DIRECTION ( 'NONE',  ( -1.000000000000000000, -1.208970125616048853E-17, 0.000000000000000000 ) ) ;
#20516 = VERTEX_POINT ( 'NONE', #954 ) ;
#20517 = CARTESIAN_POINT ( 'NONE',  ( -32.20238537491806596, -4.080045426413075660, -6.999999999999964473 ) ) ;
#20518 = AXIS2_PLACEMENT_3D ( 'NONE', #11567, #18554, #2867 ) ;
#20519 = CYLINDRICAL_SURFACE ( 'NONE', #17034, 0.9999999999999995559 ) ;
#20520 = LINE ( 'NONE', #20623, #9640 ) ;
#20521 = LINE ( 'NONE', #1496, #21907 ) ;
#20522 = EDGE_CURVE ( 'NONE', #19009, #16203, #3166, .T. ) ;
#20523 = ORIENTED_EDGE ( 'NONE', *, *, #2948, .F. ) ;
#20524 = ORIENTED_EDGE ( 'NONE', *, *, #561, .F. ) ;
#20525 = AXIS2_PLACEMENT_3D ( 'NONE', #9226, #517, #21492 ) ;
#20526 = APPLICATION_PROTOCOL_DEFINITION ( 'draft international standard', 'automotive_design', 1998, #15427 ) ;
#20527 = ORIENTED_EDGE ( 'NONE', *, *, #7041, .F. ) ;
#20528 = DIRECTION ( 'NONE',  ( 0.000000000000000000, 0.000000000000000000, 1.000000000000000000 ) ) ;
#20529 = FACE_OUTER_BOUND ( 'NONE', #20689, .T. ) ;
#20530 = AXIS2_PLACEMENT_3D ( 'NONE', #9223, #16202, #513 ) ;
#20531 = DIRECTION ( 'NONE',  ( -1.000000000000000000, -1.208970125616063644E-17, 0.000000000000000000 ) ) ;
#20532 = FACE_OUTER_BOUND ( 'NONE', #17908, .T. ) ;
#20533 = EDGE_CURVE ( 'NONE', #5024, #18296, #11942, .T. ) ;
#20534 = DIRECTION ( 'NONE',  ( 0.000000000000000000, 0.000000000000000000, 1.000000000000000000 ) ) ;
#20535 = ORIENTED_EDGE ( 'NONE', *, *, #12803, .T. ) ;
#20536 = CARTESIAN_POINT ( 'NONE',  ( -7.980461308159631173, 36.39375341857503798, -7.000000000000006217 ) ) ;
#20537 = CARTESIAN_POINT ( 'NONE',  ( -4.936596639065177428, -31.11077005834450659, -2.999999999999964473 ) ) ;
#20538 = ORIENTED_EDGE ( 'NONE', *, *, #21962, .F. ) ;
#20539 = DIRECTION ( 'NONE',  ( 0.000000000000000000, 0.000000000000000000, 1.000000000000000000 ) ) ;
#20540 = DIRECTION ( 'NONE',  ( 6.505213034913038160E-19, 3.903127820947822896E-18, 1.000000000000000000 ) ) ;
#20541 = CARTESIAN_POINT ( 'NONE',  ( 10.50000000000024514, -2.516660498395250301, -105.0010000000000048 ) ) ;
#20542 = CARTESIAN_POINT ( 'NONE',  ( -6.000000000000000000, 20.00000000000000000, -5.999999999999999112 ) ) ;
#20543 = ORIENTED_EDGE ( 'NONE', *, *, #16482, .T. ) ;
#20544 = DIRECTION ( 'NONE',  ( 0.000000000000000000, 1.000000000000000000, 0.000000000000000000 ) ) ;
#20545 = ORIENTED_EDGE ( 'NONE', *, *, #8892, .T. ) ;
#20546 = DIRECTION ( 'NONE',  ( -6.505213034913038160E-19, -3.903127820947822896E-18, -1.000000000000000000 ) ) ;
#20547 = EDGE_CURVE ( 'NONE', #21842, #17708, #18895, .T. ) ;
#20548 = CARTESIAN_POINT ( 'NONE',  ( -18.35281960068863327, 33.06122318964058593, 57.65236019522518518 ) ) ;
#20549 = ORIENTED_EDGE ( 'NONE', *, *, #19940, .F. ) ;
#20550 = DIRECTION ( 'NONE',  ( 8.659560562355143632E-17, -0.7071067811865302533, 0.7071067811865647812 ) ) ;
#20551 = AXIS2_PLACEMENT_3D ( 'NONE', #22087, #20583, #10031 ) ;
#20552 = DIRECTION ( 'NONE',  ( -0.000000000000000000, 1.000000000000000000, -0.000000000000000000 ) ) ;
#20553 = DIRECTION ( 'NONE',  ( 6.505213034913038160E-19, 3.903127820947822896E-18, 1.000000000000000000 ) ) ;
#20554 = ADVANCED_FACE ( 'NONE', ( #21592 ), #11718, .T. ) ;
#20555 = CARTESIAN_POINT ( 'NONE',  ( 17.57556337526168733, 10.44046169743542052, -57.45538260706032929 ) ) ;
#20556 = ORIENTED_EDGE ( 'NONE', *, *, #21441, .T. ) ;
#20557 = ORIENTED_EDGE ( 'NONE', *, *, #15530, .T. ) ;
#20558 = ORIENTED_EDGE ( 'NONE', *, *, #103, .T. ) ;
#20559 = ORIENTED_EDGE ( 'NONE', *, *, #18398, .F. ) ;
#20560 = DIRECTION ( 'NONE',  ( 0.000000000000000000, 1.000000000000000000, 0.000000000000000000 ) ) ;
#20561 = VECTOR ( 'NONE', #6772, 1000.000000000000114 ) ;
#20562 = LINE ( 'NONE', #22298, #19800 ) ;
#20563 = ORIENTED_EDGE ( 'NONE', *, *, #7537, .T. ) ;
#20564 = DIRECTION ( 'NONE',  ( 6.505213034913038160E-19, 3.903127820947822896E-18, 1.000000000000000000 ) ) ;
#20565 = VERTEX_POINT ( 'NONE', #22386 ) ;
#20566 = CARTESIAN_POINT ( 'NONE',  ( 2.775557561562891351E-14, -2.775557561562891351E-14, 2.999999999999995559 ) ) ;
#20567 = ORIENTED_EDGE ( 'NONE', *, *, #13759, .F. ) ;
#20568 = CARTESIAN_POINT ( 'NONE',  ( 8.970886036659246443, 37.88902356861865428, -54.67438719140665881 ) ) ;
#20569 = FACE_OUTER_BOUND ( 'NONE', #14856, .T. ) ;
#20570 = DIRECTION ( 'NONE',  ( 0.000000000000000000, -1.000000000000000000, 0.000000000000000000 ) ) ;
#20571 = CARTESIAN_POINT ( 'NONE',  ( -0.3359952163700163918, 39.99934595043738028, 48.99376255120481716 ) ) ;
#20572 = EDGE_CURVE ( 'NONE', #7317, #3415, #1630, .T. ) ;
#20573 = AXIS2_PLACEMENT_3D ( 'NONE', #4254, #11224, #18224 ) ;
#20574 = DIRECTION ( 'NONE',  ( -1.000000000000000000, -1.208970125616044077E-17, 0.000000000000000000 ) ) ;
#20575 = ORIENTED_EDGE ( 'NONE', *, *, #3224, .F. ) ;
#20576 = ORIENTED_EDGE ( 'NONE', *, *, #19289, .T. ) ;
#20577 = EDGE_CURVE ( 'NONE', #11397, #13545, #14846, .T. ) ;
#20578 = ORIENTED_EDGE ( 'NONE', *, *, #17983, .F. ) ;
#20579 = ORIENTED_EDGE ( 'NONE', *, *, #16549, .F. ) ;
#20580 = CARTESIAN_POINT ( 'NONE',  ( -22.29474960931412753, 17.42887675328155694, 58.63958600108833252 ) ) ;
#20581 = DIRECTION ( 'NONE',  ( 6.505213034913038160E-19, 3.903127820947822896E-18, 1.000000000000000000 ) ) ;
#20582 = CARTESIAN_POINT ( 'NONE',  ( 2.220446049250313081E-13, -2.498001805406602216E-13, -6.859353255829918616 ) ) ;
#20583 = DIRECTION ( 'NONE',  ( -6.505213034913038160E-19, -3.903127820947822896E-18, -1.000000000000000000 ) ) ;
#20584 = ADVANCED_FACE ( 'NONE', ( #20650 ), #4264, .F. ) ;
#20585 = VECTOR ( 'NONE', #13713, 1000.000000000000000 ) ;
#20586 = ORIENTED_EDGE ( 'NONE', *, *, #4093, .T. ) ;
#20587 = LINE ( 'NONE', #11760, #6181 ) ;
#20588 = CARTESIAN_POINT ( 'NONE',  ( -8.265432227388908260, 40.00000000000000000, -53.06731920609691855 ) ) ;
#20589 = FACE_OUTER_BOUND ( 'NONE', #20594, .T. ) ;
#20590 = CARTESIAN_POINT ( 'NONE',  ( 11.51194040402256746, 39.05862814753313472, -55.21283662269733838 ) ) ;
#20591 = EDGE_CURVE ( 'NONE', #8449, #5417, #14497, .T. ) ;
#20592 = ORIENTED_EDGE ( 'NONE', *, *, #11267, .F. ) ;
#20593 = DIRECTION ( 'NONE',  ( -1.000000000000000000, 0.000000000000000000, 0.000000000000000000 ) ) ;
#20594 = EDGE_LOOP ( 'NONE', ( #8968, #9219, #7864, #4717 ) ) ;
#20595 = CARTESIAN_POINT ( 'NONE',  ( 5.551115123125782702E-14, -1.387778780781445676E-13, -5.749999999999949374 ) ) ;
#20596 = CYLINDRICAL_SURFACE ( 'NONE', #16643, 2.500000000000002220 ) ;
#20597 = DIRECTION ( 'NONE',  ( 6.505213034913038160E-19, 3.903127820947822896E-18, 1.000000000000000000 ) ) ;
#20598 = EDGE_LOOP ( 'NONE', ( #1965, #1023, #20490, #4471 ) ) ;
#20599 = CIRCLE ( 'NONE', #10703, 2.500000000000002220 ) ;
#20600 = CIRCLE ( 'NONE', #22447, 19.11328065563150957 ) ;
#20601 = ORIENTED_EDGE ( 'NONE', *, *, #9671, .T. ) ;
#20602 = CARTESIAN_POINT ( 'NONE',  ( 42.50000000000000711, -5.000000000000000000, 45.40000000000001279 ) ) ;
#20603 = CARTESIAN_POINT ( 'NONE',  ( -14.76298474240507552, -28.95348479018572263, 3.000000000000023537 ) ) ;
#20604 = ORIENTED_EDGE ( 'NONE', *, *, #19008, .T. ) ;
#20605 = EDGE_CURVE ( 'NONE', #13471, #8183, #20377, .T. ) ;
#20606 = FACE_OUTER_BOUND ( 'NONE', #3758, .T. ) ;
#20607 = DIRECTION ( 'NONE',  ( 1.000000000000000000, -0.000000000000000000, -1.445602896647339163E-16 ) ) ;
#20608 = DIRECTION ( 'NONE',  ( -0.000000000000000000, 1.000000000000000000, -0.000000000000000000 ) ) ;
#20609 = CARTESIAN_POINT ( 'NONE',  ( -19.93949378746062351, 21.61607484719041850, -60.60748883510625973 ) ) ;
#20610 = CARTESIAN_POINT ( 'NONE',  ( -9.852267639826653323, 31.31642578264289156, -43.21671877549178475 ) ) ;
#20611 = ADVANCED_FACE ( 'NONE', ( #15025 ), #15476, .T. ) ;
#20612 = AXIS2_PLACEMENT_3D ( 'NONE', #137, #7132, #15825 ) ;
#20613 = FACE_OUTER_BOUND ( 'NONE', #9346, .T. ) ;
#20614 = ORIENTED_EDGE ( 'NONE', *, *, #21786, .F. ) ;
#20615 = CARTESIAN_POINT ( 'NONE',  ( 7.017626609043924546, 33.27455722914837111, 41.44244536674933954 ) ) ;
#20616 = LINE ( 'NONE', #15680, #15142 ) ;
#20617 = CIRCLE ( 'NONE', #13644, 19.11328065563152023 ) ;
#20618 = CARTESIAN_POINT ( 'NONE',  ( 9.103081159019511759, 0.03030367950603989405, -53.87333532811885561 ) ) ;
#20619 = CARTESIAN_POINT ( 'NONE',  ( 6.742883674876798850, 34.24928931925766307, 2.999999999999999112 ) ) ;
#20620 = CIRCLE ( 'NONE', #14750, 1.000000000000001776 ) ;
#20621 = ORIENTED_EDGE ( 'NONE', *, *, #3732, .F. ) ;
#20622 = DIRECTION ( 'NONE',  ( 1.000000000000000000, 0.000000000000000000, 0.000000000000000000 ) ) ;
#20623 = CARTESIAN_POINT ( 'NONE',  ( 35.00000000000000711, -4.999999999999997335, -57.00000000000001421 ) ) ;
#20624 = CIRCLE ( 'NONE', #13654, 17.00000000000000355 ) ;
#20625 = EDGE_CURVE ( 'NONE', #3760, #22096, #6788, .T. ) ;
#20626 = VERTEX_POINT ( 'NONE', #22043 ) ;
#20627 = AXIS2_PLACEMENT_3D ( 'NONE', #17955, #772, #9486 ) ;
#20628 = CIRCLE ( 'NONE', #875, 19.11328065563150957 ) ;
#20629 = APPLICATION_PROTOCOL_DEFINITION ( 'draft international standard', 'automotive_design', 1998, #14996 ) ;
#20630 = EDGE_CURVE ( 'NONE', #15727, #18296, #12058, .T. ) ;
#20631 = ADVANCED_FACE ( 'NONE', ( #16879 ), #10214, .F. ) ;
#20632 = COLOUR_RGB ( '',0.7921568627450980005, 0.8196078431372548767, 0.9333333333333333481 ) ;
#20633 = VERTEX_POINT ( 'NONE', #4630 ) ;
#20634 = CARTESIAN_POINT ( 'NONE',  ( 31.57187188083540619, 7.711478842616415363, -7.000000000000006217 ) ) ;
#20635 = CARTESIAN_POINT ( 'NONE',  ( 36.75746821813321930, -0.6841746959067585010, -2.800654218530457484 ) ) ;
#20636 = DIRECTION ( 'NONE',  ( -1.000000000000000000, 0.000000000000000000, 0.000000000000000000 ) ) ;
#20637 = FACE_OUTER_BOUND ( 'NONE', #2749, .T. ) ;
#20638 = CARTESIAN_POINT ( 'NONE',  ( -35.00000000000000000, 40.00000000000000000, -49.99999999999997158 ) ) ;
#20639 = EDGE_LOOP ( 'NONE', ( #3250, #15290, #22617, #10224 ) ) ;
#20640 = DIRECTION ( 'NONE',  ( 0.000000000000000000, -1.000000000000000000, 0.000000000000000000 ) ) ;
#20641 = CARTESIAN_POINT ( 'NONE',  ( 35.00000000000000000, -5.000000000000000000, 52.49999999999698019 ) ) ;
#20642 = ORIENTED_EDGE ( 'NONE', *, *, #6978, .T. ) ;
#20643 = LINE ( 'NONE', #15702, #18565 ) ;
#20644 = CYLINDRICAL_SURFACE ( 'NONE', #19617, 19.11328065563150957 ) ;
#20645 = CARTESIAN_POINT ( 'NONE',  ( -35.00000000000000000, -4.928932188134504955, 1.387778780781445676E-14 ) ) ;
#20646 = CARTESIAN_POINT ( 'NONE',  ( 7.766910979104990176, 39.99999999999999289, 52.87044925761806269 ) ) ;
#20647 = ORIENTED_EDGE ( 'NONE', *, *, #6511, .F. ) ;
#20648 = DIRECTION ( 'NONE',  ( -1.000000000000000000, -1.208970125616060717E-17, 0.000000000000000000 ) ) ;
#20649 = ORIENTED_EDGE ( 'NONE', *, *, #12181, .T. ) ;
#20650 = FACE_OUTER_BOUND ( 'NONE', #9455, .T. ) ;
#20651 = CIRCLE ( 'NONE', #21387, 6.499999999999999112 ) ;
#20652 = CARTESIAN_POINT ( 'NONE',  ( -21.73016838732310774, 25.62687619368171710, 58.51481333197136792 ) ) ;
#20653 = ORIENTED_EDGE ( 'NONE', *, *, #15050, .F. ) ;
#20654 = DIRECTION ( 'NONE',  ( 0.000000000000000000, 0.000000000000000000, 1.000000000000000000 ) ) ;
#20655 = AXIS2_PLACEMENT_3D ( 'NONE', #10842, #21742, #6039 ) ;
#20656 = LINE ( 'NONE', #4753, #10798 ) ;
#20657 = CARTESIAN_POINT ( 'NONE',  ( 1.128083539116558898, 34.88850421923955736, 3.000000000000002665 ) ) ;
#20658 = VECTOR ( 'NONE', #8614, 1000.000000000000227 ) ;
#20659 = PLANE ( 'NONE',  #6743 ) ;
#20660 = EDGE_CURVE ( 'NONE', #599, #15249, #1176, .T. ) ;
#20661 = ORIENTED_EDGE ( 'NONE', *, *, #6109, .F. ) ;
#20662 = VERTEX_POINT ( 'NONE', #1407 ) ;
#20663 = CONICAL_SURFACE ( 'NONE', #11156, 2.099999999999997868, 1.029744258676652091 ) ;
#20664 = ORIENTED_EDGE ( 'NONE', *, *, #9439, .F. ) ;
#20666 = ADVANCED_FACE ( 'NONE', ( #8396 ), #6675, .T. ) ;
#20665 = DIRECTION ( 'NONE',  ( -1.296372316667914327E-16, -1.000000000000000000, 0.000000000000000000 ) ) ;
#20667 = EDGE_CURVE ( 'NONE', #15820, #17279, #15966, .T. ) ;
#20668 = EDGE_CURVE ( 'NONE', #6975, #19682, #18604, .T. ) ;
#20669 = ORIENTED_EDGE ( 'NONE', *, *, #19789, .T. ) ;
#20670 = LINE ( 'NONE', #13983, #13246 ) ;
#20671 = AXIS2_PLACEMENT_3D ( 'NONE', #4462, #2398, #7894 ) ;
#20672 = CARTESIAN_POINT ( 'NONE',  ( 22.41121774633936070, 19.23761757294737151, 58.66449182057562695 ) ) ;
#20673 = DIRECTION ( 'NONE',  ( -0.000000000000000000, -1.000000000000000000, -0.000000000000000000 ) ) ;
#20674 = ORIENTED_EDGE ( 'NONE', *, *, #9181, .F. ) ;
#20675 = CARTESIAN_POINT ( 'NONE',  ( -34.99999999999999289, 4.000000000000028422, -10.00000000000003020 ) ) ;
#20676 = DIRECTION ( 'NONE',  ( 0.000000000000000000, 0.000000000000000000, 1.000000000000000000 ) ) ;
#20677 = ORIENTED_EDGE ( 'NONE', *, *, #3927, .T. ) ;
#20678 = ORIENTED_EDGE ( 'NONE', *, *, #19033, .F. ) ;
#20679 = CYLINDRICAL_SURFACE ( 'NONE', #957, 2.099999999999997868 ) ;
#20680 = ADVANCED_FACE ( 'NONE', ( #8281 ), #16339, .T. ) ;
#20681 = DIRECTION ( 'NONE',  ( 1.000000000000000000, 0.000000000000000000, 0.000000000000000000 ) ) ;
#20682 = AXIS2_PLACEMENT_3D ( 'NONE', #619, #14919, #20215 ) ;
#20683 = DIRECTION ( 'NONE',  ( 0.000000000000000000, 0.000000000000000000, 1.000000000000000000 ) ) ;
#20684 = CARTESIAN_POINT ( 'NONE',  ( -5.724874953890430440, 39.79387174624774559, 52.64592308926970077 ) ) ;
#20685 = VECTOR ( 'NONE', #8315, 1000.000000000000000 ) ;
#20686 = DIRECTION ( 'NONE',  ( 0.000000000000000000, -1.000000000000000000, 0.000000000000000000 ) ) ;
#20687 = VECTOR ( 'NONE', #8609, 1000.000000000000000 ) ;
#20688 = DIRECTION ( 'NONE',  ( -6.505213034913038160E-19, -3.903127820947822896E-18, -1.000000000000000000 ) ) ;
#20689 = EDGE_LOOP ( 'NONE', ( #16364, #12761, #11278, #12374 ) ) ;
#20690 = ORIENTED_EDGE ( 'NONE', *, *, #4026, .F. ) ;
#20691 =( BOUNDED_SURFACE ( )  B_SPLINE_SURFACE ( 3, 2, ( 
 ( #22094, #4450, #14627 ),
 ( #2620, #12900, #9492 ),
 ( #19911, #9829, #6168 ),
 ( #16817, #2844, #6045 ),
 ( #21869, #13235, #21634 ),
 ( #13133, #21986, #7761 ),
 ( #18411, #16580, #14961 ),
 ( #887, #1121, #4217 ),
 ( #8114, #14733, #20148 ),
 ( #11427, #16472, #18068 ),
 ( #2731, #6277, #9710 ),
 ( #11078, #2384, #5930 ),
 ( #15072, #16700, #9377 ),
 ( #7656, #4108, #1003 ) ),
 .UNSPECIFIED., .F., .F., .F. ) 
 B_SPLINE_SURFACE_WITH_KNOTS ( ( 4, 2, 2, 2, 2, 2, 4 ),
 ( 3, 3 ),
 ( 0.004259382447192780127, 0.005809352080732721121, 0.007359321714272661248, 0.008909291347812601375, 0.01045926098135254237, 0.01355920024843242262, 0.01665913951551230288 ),
 ( 0.000000000000000000, 0.8363210495138897471 ),
 .UNSPECIFIED. ) 
 GEOMETRIC_REPRESENTATION_ITEM ( )  RATIONAL_B_SPLINE_SURFACE ( (
 ( 1.000000000000000000, 0.7012738381899416007, 0.9022096307043713237),
 ( 1.000000000000000000, 0.7322964233739771567, 0.9123651190729491489),
 ( 1.000000000000000000, 0.7591992615145440881, 0.9211719756968406170),
 ( 1.000000000000000000, 0.8072864693883526899, 0.9369137031300254215),
 ( 1.000000000000000000, 0.8284610246205110773, 0.9438453610848451802),
 ( 1.000000000000000000, 0.8663819189607202542, 0.9562590654590453765),
 ( 1.000000000000000000, 0.8831517595277805777, 0.9617488052667169107),
 ( 1.000000000000000000, 0.9127683925939877874, 0.9714440441011351624),
 ( 1.000000000000000000, 0.9255808901573298053, 0.9756383164096822380),
 ( 1.000000000000000000, 0.9589862157102829743, 0.9865738136639907729),
 ( 1.000000000000000000, 0.9746015990832553877, 0.9916856327878436073),
 ( 1.000000000000000000, 0.9951270141023534910, 0.9984047895650791649),
 ( 1.000000000000000000, 0.9999818006517211533, 0.9999940422995483580),
 ( 1.000000000000000000, 1.000000000000000000, 1.000000000000000000) ) ) 
 REPRESENTATION_ITEM ( '' )  SURFACE ( )  );
#20692 = ORIENTED_EDGE ( 'NONE', *, *, #19658, .T. ) ;
#20693 = AXIS2_PLACEMENT_3D ( 'NONE', #12601, #18339, #587 ) ;
#20694 = ORIENTED_EDGE ( 'NONE', *, *, #16216, .T. ) ;
#20695 = DIRECTION ( 'NONE',  ( 6.505213034913038160E-19, 3.903127820947822896E-18, 1.000000000000000000 ) ) ;
#20696 = CARTESIAN_POINT ( 'NONE',  ( -12.11890052765076220, 39.66666666666666430, 54.74394698394426229 ) ) ;
#20697 = AXIS2_PLACEMENT_3D ( 'NONE', #5738, #9519, #2187 ) ;
#20698 = FACE_OUTER_BOUND ( 'NONE', #11913, .T. ) ;
#20699 = AXIS2_PLACEMENT_3D ( 'NONE', #2328, #12621, #4168 ) ;
#20700 = CARTESIAN_POINT ( 'NONE',  ( -11.73108507413472346, 40.00000000000000000, 54.23086838360213591 ) ) ;
#20701 = ADVANCED_FACE ( 'NONE', ( #16981 ), #13531, .F. ) ;
#20702 = EDGE_CURVE ( 'NONE', #9840, #22614, #10100, .T. ) ;
#20703 = ORIENTED_EDGE ( 'NONE', *, *, #2630, .T. ) ;
#20704 = DIRECTION ( 'NONE',  ( 6.505213034913038160E-19, 3.903127820947822896E-18, 1.000000000000000000 ) ) ;
#20705 = DIRECTION ( 'NONE',  ( -0.000000000000000000, 1.000000000000000000, -0.000000000000000000 ) ) ;
#20706 = DIRECTION ( 'NONE',  ( 6.505213034913038160E-19, 3.903127820947822896E-18, 1.000000000000000000 ) ) ;
#20707 = PLANE ( 'NONE',  #4612 ) ;
#20708 = SURFACE_STYLE_FILL_AREA ( #3648 ) ;
#20709 = VERTEX_POINT ( 'NONE', #1748 ) ;
#20710 = CYLINDRICAL_SURFACE ( 'NONE', #7585, 1.000000000000000888 ) ;
#20711 = EDGE_CURVE ( 'NONE', #22326, #15589, #21087, .T. ) ;
#20712 = DIRECTION ( 'NONE',  ( 0.000000000000000000, -1.000000000000000000, 0.000000000000000000 ) ) ;
#20713 = AXIS2_PLACEMENT_3D ( 'NONE', #11372, #9546, #13072 ) ;
#20714 = EDGE_LOOP ( 'NONE', ( #9446, #5403, #8604, #19736, #4418, #11861, #15878, #11214 ) ) ;
#20715 = CARTESIAN_POINT ( 'NONE',  ( -24.03323817228460157, 20.36304159388333090, -2.999999999999988898 ) ) ;
#20716 = AXIS2_PLACEMENT_3D ( 'NONE', #21850, #11058, #4544 ) ;
#20717 = CARTESIAN_POINT ( 'NONE',  ( -47.83731665821552781, 10.00000000000000000, -38.93845529828707441 ) ) ;
#20718 = DIRECTION ( 'NONE',  ( -1.000000000000000000, 0.000000000000000000, 0.000000000000000000 ) ) ;
#20719 = PLANE ( 'NONE',  #17044 ) ;
#20720 = EDGE_LOOP ( 'NONE', ( #15971, #6814, #2090, #11645 ) ) ;
#20721 = AXIS2_PLACEMENT_3D ( 'NONE', #20273, #18206, #11208 ) ;
#20722 = B_SPLINE_CURVE_WITH_KNOTS ( 'NONE', 3,
 ( #12716, #11118, #21668, #19738 ),
 .UNSPECIFIED., .F., .F.,
 ( 4, 4 ),
 ( 0.001893031756885608539, 0.003808480026563944992 ),
 .UNSPECIFIED. ) ;
#20723 = ORIENTED_EDGE ( 'NONE', *, *, #7070, .T. ) ;
#20724 = CARTESIAN_POINT ( 'NONE',  ( -3.192088256997320350, -4.645848710072370658, 47.73628783182301305 ) ) ;
#20725 = EDGE_CURVE ( 'NONE', #4439, #454, #971, .T. ) ;
#20726 = CARTESIAN_POINT ( 'NONE',  ( 35.00000000000000000, -9.000000000000001776, -9.000000000000000000 ) ) ;
#20727 = CIRCLE ( 'NONE', #10416, 60.00000000000000000 ) ;
#20728 = TOROIDAL_SURFACE ( 'NONE', #13011, 50.00000000000000000, 10.00000000000000000 ) ;
#20729 = AXIS2_PLACEMENT_3D ( 'NONE', #4958, #9987, #20439 ) ;
#20730 = ORIENTED_EDGE ( 'NONE', *, *, #6475, .F. ) ;
#20731 = AXIS2_PLACEMENT_3D ( 'NONE', #3620, #19197, #152 ) ;
#20732 = CARTESIAN_POINT ( 'NONE',  ( 9.579024991656979182, 8.451577327321064814, 43.05667825653220149 ) ) ;
#20733 = CARTESIAN_POINT ( 'NONE',  ( -2.090752864397128707, 34.85582703520299930, -38.95144853163190390 ) ) ;
#20734 = DIRECTION ( 'NONE',  ( 0.000000000000000000, 0.000000000000000000, 1.000000000000000000 ) ) ;
#20735 = CARTESIAN_POINT ( 'NONE',  ( -18.87679372942798395, 13.33229001579394968, -60.34430474298741842 ) ) ;
#20736 = CARTESIAN_POINT ( 'NONE',  ( -6.629162819447105726, 39.71713125805204214, 53.15137286438373820 ) ) ;
#20737 = AXIS2_PLACEMENT_3D ( 'NONE', #6263, #13223, #11066 ) ;
#20738 = ORIENTED_EDGE ( 'NONE', *, *, #16714, .F. ) ;
#20739 = CARTESIAN_POINT ( 'NONE',  ( 14.98515767422208178, 20.77155976913489610, 45.81928800960653803 ) ) ;
#20740 =( LENGTH_UNIT ( ) NAMED_UNIT ( * ) SI_UNIT ( .MILLI., .METRE. ) );
#20741 = CARTESIAN_POINT ( 'NONE',  ( -13.85640646055084702, -25.00000000000000000, 7.999999999999705125 ) ) ;
#20742 = CARTESIAN_POINT ( 'NONE',  ( 6.953913411055066440, 34.84300730320191519, 3.000000000000042188 ) ) ;
#20743 = EDGE_LOOP ( 'NONE', ( #17090, #19622, #6547, #12364 ) ) ;
#20744 = DIRECTION ( 'NONE',  ( 0.000000000000000000, 0.000000000000000000, -1.000000000000000000 ) ) ;
#20745 = CYLINDRICAL_SURFACE ( 'NONE', #8921, 4.999999999999997335 ) ;
#20746 = CARTESIAN_POINT ( 'NONE',  ( -35.00000000000000000, 22.00000000000000711, -14.99999999999997691 ) ) ;
#20747 = CIRCLE ( 'NONE', #21852, 57.00000000000002132 ) ;
#20748 = EDGE_CURVE ( 'NONE', #8849, #22077, #5404, .T. ) ;
#20749 = ORIENTED_EDGE ( 'NONE', *, *, #15734, .T. ) ;
#20750 = EDGE_CURVE ( 'NONE', #5360, #13935, #13755, .T. ) ;
#20751 = APPLICATION_PROTOCOL_DEFINITION ( 'draft international standard', 'automotive_design', 1998, #17787 ) ;
#20752 = EDGE_LOOP ( 'NONE', ( #8499, #20342, #10078, #10211 ) ) ;
#20753 = FACE_OUTER_BOUND ( 'NONE', #6463, .T. ) ;
#20754 = FACE_OUTER_BOUND ( 'NONE', #2567, .T. ) ;
#20755 = CARTESIAN_POINT ( 'NONE',  ( 35.00000000000000000, 38.99999999999999289, 4.258610482196280173E-15 ) ) ;
#20756 = CARTESIAN_POINT ( 'NONE',  ( -22.26748298433250994, 22.28024240313478188, -6.999999999999957367 ) ) ;
#20757 = VECTOR ( 'NONE', #21585, 1000.000000000000000 ) ;
#20758 = EDGE_LOOP ( 'NONE', ( #12762, #17779, #3933, #3978, #1073, #3843 ) ) ;
#20759 = CARTESIAN_POINT ( 'NONE',  ( -21.00948735876860596, -24.79619811426211839, 2.999999999999995559 ) ) ;
#20760 = CARTESIAN_POINT ( 'NONE',  ( -34.99999999999980815, 28.00000000000000000, 54.99999999999922551 ) ) ;
#20761 = EDGE_LOOP ( 'NONE', ( #6056, #7899, #21902, #6624 ) ) ;
#20762 = DIRECTION ( 'NONE',  ( 0.000000000000000000, 0.000000000000000000, 1.000000000000000000 ) ) ;
#20763 = AXIS2_PLACEMENT_3D ( 'NONE', #14398, #18195, #21755 ) ;
#20764 = DIRECTION ( 'NONE',  ( -1.000000000000000000, 0.000000000000000000, 0.000000000000000000 ) ) ;
#20765 = DIRECTION ( 'NONE',  ( 1.000000000000000000, 1.208970125616067188E-17, 0.000000000000000000 ) ) ;
#20766 = CARTESIAN_POINT ( 'NONE',  ( 9.066530173131811310, 39.99999999999999289, 53.36211915552348728 ) ) ;
#20767 = CARTESIAN_POINT ( 'NONE',  ( 35.00000000000000000, 10.00000000000000000, 41.00000000000002132 ) ) ;
#20768 = EDGE_CURVE ( 'NONE', #8398, #573, #13392, .T. ) ;
#20769 = ORIENTED_EDGE ( 'NONE', *, *, #10691, .F. ) ;
#20770 = DIRECTION ( 'NONE',  ( 0.000000000000000000, -1.000000000000000000, 0.000000000000000000 ) ) ;
#20771 = CARTESIAN_POINT ( 'NONE',  ( -22.43696576003033982, 20.17999529786816737, 58.67002796852977298 ) ) ;
#20772 = ORIENTED_EDGE ( 'NONE', *, *, #13320, .F. ) ;
#20773 = FACE_OUTER_BOUND ( 'NONE', #9512, .T. ) ;
#20774 = VECTOR ( 'NONE', #14071, 1000.000000000000000 ) ;
#20775 = CIRCLE ( 'NONE', #2106, 5.000000000000000000 ) ;
#20776 = FACE_OUTER_BOUND ( 'NONE', #19001, .T. ) ;
#20777 = DIRECTION ( 'NONE',  ( 1.049727191138617217E-16, 0.5150380749100562650, -0.8571673007021111124 ) ) ;
#20778 = ADVANCED_FACE ( 'NONE', ( #17889 ), #19998, .T. ) ;
#20779 = DIRECTION ( 'NONE',  ( -1.000000000000000000, 0.000000000000000000, 0.000000000000000000 ) ) ;
#20780 = VECTOR ( 'NONE', #16118, 1000.000000000000000 ) ;
#20781 = AXIS2_PLACEMENT_3D ( 'NONE', #18062, #20026, #21517 ) ;
#20782 = VERTEX_POINT ( 'NONE', #7014 ) ;
#20783 = EDGE_CURVE ( 'NONE', #9047, #9571, #13971, .T. ) ;
#20784 = ORIENTED_EDGE ( 'NONE', *, *, #1051, .F. ) ;
#20785 = ORIENTED_EDGE ( 'NONE', *, *, #5445, .F. ) ;
#20786 = LINE ( 'NONE', #19178, #12025 ) ;
#20787 = ORIENTED_EDGE ( 'NONE', *, *, #15942, .F. ) ;
#20788 = DIRECTION ( 'NONE',  ( -1.000000000000000000, -1.208970125616060101E-17, 6.505213034913038160E-19 ) ) ;
#20789 = CARTESIAN_POINT ( 'NONE',  ( 1.102182119232617517E-15, 28.49999999999998934, 8.999999999999998224 ) ) ;
#20790 = DIRECTION ( 'NONE',  ( 0.000000000000000000, 1.000000000000000000, 0.000000000000000000 ) ) ;
#20791 = ORIENTED_EDGE ( 'NONE', *, *, #21328, .T. ) ;
#20792 = CARTESIAN_POINT ( 'NONE',  ( 29.74882400976413876, 20.54749497201894570, 2.932969818539052476 ) ) ;
#20793 = PLANE ( 'NONE',  #1864 ) ;
#20794 = ORIENTED_EDGE ( 'NONE', *, *, #12957, .F. ) ;
#20795 = CIRCLE ( 'NONE', #17854, 18.00000000000000000 ) ;
#20796 = CYLINDRICAL_SURFACE ( 'NONE', #179, 41.00000000000000000 ) ;
#20797 = EDGE_CURVE ( 'NONE', #9047, #22397, #5724, .T. ) ;
#20798 = CARTESIAN_POINT ( 'NONE',  ( 5.833333333333338366, 33.81926995981415729, 40.61164310337067462 ) ) ;
#20799 = ORIENTED_EDGE ( 'NONE', *, *, #9040, .T. ) ;
#20800 = CARTESIAN_POINT ( 'NONE',  ( 6.803227178530688590, 38.81166136533672528, -55.43135129401763805 ) ) ;
#20801 = VECTOR ( 'NONE', #19449, 1000.000000000000114 ) ;
#20802 = DIRECTION ( 'NONE',  ( 1.296372316667914327E-16, 1.000000000000000000, -0.000000000000000000 ) ) ;
#20803 = DIRECTION ( 'NONE',  ( -6.505213034913038160E-19, -3.903127820947822896E-18, -1.000000000000000000 ) ) ;
#20804 = AXIS2_PLACEMENT_3D ( 'NONE', #13915, #19332, #1800 ) ;
#20805 = CARTESIAN_POINT ( 'NONE',  ( -0.5387139470867652324, 39.99828243297760366, 49.14868387071282996 ) ) ;
#20806 = CARTESIAN_POINT ( 'NONE',  ( 18.13678767552818272, 6.731837175187128430, 57.58481432322350457 ) ) ;
#20807 = CYLINDRICAL_SURFACE ( 'NONE', #4505, 2.499999999999995115 ) ;
#20808 = ADVANCED_FACE ( 'NONE', ( #12482 ), #19496, .F. ) ;
#20809 = CARTESIAN_POINT ( 'NONE',  ( -0.6841746959067307454, -36.75746821813308429, 2.800654218530485018 ) ) ;
#20810 = CIRCLE ( 'NONE', #3982, 58.99999999999702283 ) ;
#20811 = ORIENTED_EDGE ( 'NONE', *, *, #6400, .F. ) ;
#20812 = CIRCLE ( 'NONE', #10915, 58.99999999999699440 ) ;
#20813 = AXIS2_PLACEMENT_3D ( 'NONE', #779, #4449, #14732 ) ;
#20814 = ORIENTED_EDGE ( 'NONE', *, *, #218, .T. ) ;
#20815 = EDGE_CURVE ( 'NONE', #14096, #5340, #6091, .T. ) ;
#20816 = ORIENTED_EDGE ( 'NONE', *, *, #6261, .T. ) ;
#20817 = AXIS2_PLACEMENT_3D ( 'NONE', #1847, #9280, #8827 ) ;
#20818 = EDGE_LOOP ( 'NONE', ( #7595, #7035, #3373, #19456 ) ) ;
#20819 = DIRECTION ( 'NONE',  ( -0.000000000000000000, 1.000000000000000000, -0.000000000000000000 ) ) ;
#20820 = CARTESIAN_POINT ( 'NONE',  ( -11.85401191286884703, -32.83234229683740324, -2.999999999999971578 ) ) ;
#20821 = EDGE_CURVE ( 'NONE', #6579, #6323, #21464, .T. ) ;
#20822 = CARTESIAN_POINT ( 'NONE',  ( -3.435937872931129410E-14, -0.6657802223429154509, 48.32248901598323698 ) ) ;
#20823 = CARTESIAN_POINT ( 'NONE',  ( 6.069328058468995479, 39.76463894486199990, 52.83839005242463571 ) ) ;
#20824 = EDGE_CURVE ( 'NONE', #1508, #17625, #7178, .T. ) ;
#20825 = AXIS2_PLACEMENT_3D ( 'NONE', #17605, #22678, #3530 ) ;
#20826 = ORIENTED_EDGE ( 'NONE', *, *, #11189, .F. ) ;
#20827 = DIRECTION ( 'NONE',  ( -6.505213034913038160E-19, -3.903127820947822896E-18, -1.000000000000000000 ) ) ;
#20828 = CARTESIAN_POINT ( 'NONE',  ( -35.00000000000000000, 2.142135623730931471, 1.387778780781445676E-14 ) ) ;
#20829 = TOROIDAL_SURFACE ( 'NONE', #9845, 34.90673715956759082, 8.750000000000000000 ) ;
#20830 = DIRECTION ( 'NONE',  ( 6.505213034913038160E-19, 3.903127820947822896E-18, 1.000000000000000000 ) ) ;
#20831 = CARTESIAN_POINT ( 'NONE',  ( 10.06223851446537410, 39.28158160658947651, -54.67678195792276341 ) ) ;
#20832 = PRESENTATION_STYLE_ASSIGNMENT (( #14026 ) ) ;
#20833 = ORIENTED_EDGE ( 'NONE', *, *, #10630, .F. ) ;
#20834 = CARTESIAN_POINT ( 'NONE',  ( 17.32050807568869644, -1.500000000000011768, 10.00000000000013323 ) ) ;
#20835 = CARTESIAN_POINT ( 'NONE',  ( -20.00000000000001421, 20.00000000000000355, 60.62177826491070931 ) ) ;
#20836 = AXIS2_PLACEMENT_3D ( 'NONE', #7805, #21799, #6314 ) ;
#20837 = ORIENTED_EDGE ( 'NONE', *, *, #7245, .F. ) ;
#20838 = CARTESIAN_POINT ( 'NONE',  ( -32.40961249803532240, 2.422192751863644133, -6.999999999999950262 ) ) ;
#20839 = CARTESIAN_POINT ( 'NONE',  ( -8.970889523128901644, 37.88902197091756818, 54.67437798809974225 ) ) ;
#20840 = CARTESIAN_POINT ( 'NONE',  ( -30.07487443287959650, 12.31876324338271367, -2.999999999999999112 ) ) ;
#20841 = DIRECTION ( 'NONE',  ( -1.000000000000000000, -1.788446540656407544E-15, 0.000000000000000000 ) ) ;
#20842 = EDGE_CURVE ( 'NONE', #4303, #21260, #3801, .T. ) ;
#20843 = ORIENTED_EDGE ( 'NONE', *, *, #19319, .T. ) ;
#20844 = ADVANCED_FACE ( 'NONE', ( #3472 ), #10545, .F. ) ;
#20845 = ORIENTED_EDGE ( 'NONE', *, *, #15606, .T. ) ;
#20846 = AXIS2_PLACEMENT_3D ( 'NONE', #11459, #14461, #7271 ) ;
#20847 = VERTEX_POINT ( 'NONE', #3918 ) ;
#20848 = CARTESIAN_POINT ( 'NONE',  ( 35.00000000000001421, -5.000000000000000000, 59.99999999999703704 ) ) ;
#20849 = EDGE_CURVE ( 'NONE', #1702, #10048, #681, .T. ) ;
#20850 = DIRECTION ( 'NONE',  ( 0.000000000000000000, -1.000000000000000000, 0.000000000000000000 ) ) ;
#20851 = ORIENTED_EDGE ( 'NONE', *, *, #3649, .T. ) ;
#20852 = DIRECTION ( 'NONE',  ( 0.000000000000000000, 1.000000000000000000, 0.000000000000000000 ) ) ;
#20853 = CARTESIAN_POINT ( 'NONE',  ( 13.83143812983109200, -29.36548507648034700, 3.000000000000023537 ) ) ;
#20854 = DIRECTION ( 'NONE',  ( 0.000000000000000000, -1.000000000000000000, 0.000000000000000000 ) ) ;
#20855 = CARTESIAN_POINT ( 'NONE',  ( -19.27384183542242369, 25.35969264784100474, -57.95172789105616573 ) ) ;
#20856 = LINE ( 'NONE', #8581, #8244 ) ;
#20857 = ORIENTED_EDGE ( 'NONE', *, *, #14778, .F. ) ;
#20858 = DIRECTION ( 'NONE',  ( -1.296372316667914327E-16, -1.000000000000000000, 0.000000000000000000 ) ) ;
#20859 = CARTESIAN_POINT ( 'NONE',  ( 1.128083539116392364, 34.88850421923958578, -2.999999999999981792 ) ) ;
#20860 = FACE_OUTER_BOUND ( 'NONE', #17814, .T. ) ;
#20861 = ORIENTED_EDGE ( 'NONE', *, *, #17490, .T. ) ;
#20862 = CARTESIAN_POINT ( 'NONE',  ( 27.57461708434214032, -4.862148974673824675, -2.999999999999971578 ) ) ;
#20863 = CARTESIAN_POINT ( 'NONE',  ( -10.39230484541309174, 1.500000000000008216, 5.999999999999708677 ) ) ;
#20864 = EDGE_CURVE ( 'NONE', #10675, #8683, #14314, .T. ) ;
#20865 = AXIS2_PLACEMENT_3D ( 'NONE', #17982, #13153, #2529 ) ;
#20866 = VERTEX_POINT ( 'NONE', #8613 ) ;
#20867 = CIRCLE ( 'NONE', #16829, 1.000000000000000888 ) ;
#20868 = EDGE_CURVE ( 'NONE', #16771, #2945, #1858, .T. ) ;
#20869 = ORIENTED_EDGE ( 'NONE', *, *, #19445, .F. ) ;
#20870 = DIRECTION ( 'NONE',  ( 6.505213034913038160E-19, 3.903127820947822896E-18, 1.000000000000000000 ) ) ;
#20871 = LINE ( 'NONE', #10081, #12832 ) ;
#20872 = CARTESIAN_POINT ( 'NONE',  ( -89.99999999999701572, -5.000000000000000000, -3.012171160963566127E-14 ) ) ;
#20873 = FACE_OUTER_BOUND ( 'NONE', #9525, .T. ) ;
#20874 = CARTESIAN_POINT ( 'NONE',  ( -28.07080038625074536, -14.29266125237910146, 2.999999999999995559 ) ) ;
#20875 = EDGE_LOOP ( 'NONE', ( #17194, #1329 ) ) ;
#20876 = FACE_OUTER_BOUND ( 'NONE', #6245, .T. ) ;
#20877 = DIRECTION ( 'NONE',  ( -1.000000000000000000, 0.000000000000000000, 0.000000000000000000 ) ) ;
#20878 = ORIENTED_EDGE ( 'NONE', *, *, #8470, .F. ) ;
#20879 = CARTESIAN_POINT ( 'NONE',  ( 4.084299015953619438, -4.682619376883208950, -48.27507093818998385 ) ) ;
#20880 = B_SPLINE_CURVE_WITH_KNOTS ( 'NONE', 3,
 ( #21791, #7577, #21566, #6087, #5867, #2428, #9632, #13051, #4377, #12721, #12830, #711, #11355, #7693, #1045, #16622, #14882, #14670, #929, #21908, #6204, #13166 ),
 .UNSPECIFIED., .F., .F.,
 ( 4, 2, 2, 2, 2, 2, 2, 2, 2, 2, 4 ),
 ( 0.007712149587921343294, 0.01231940472852627484, 0.01347121851367750339, 0.01462303229882873194, 0.01692665986913119425, 0.01807847365428242800, 0.01923028743943366176, 0.02153391500973612233, 0.02268572879488734914, 0.02383754258003857596, 0.02614117015034102959 ),
 .UNSPECIFIED. ) ;
#20881 = EDGE_CURVE ( 'NONE', #11692, #8817, #7190, .T. ) ;
#20882 = CARTESIAN_POINT ( 'NONE',  ( 20.89512770937650643, 28.22558907592241084, -58.31975796628788089 ) ) ;
#20883 =( REPRESENTATION_RELATIONSHIP ('NONE','NONE', #8442, #21420 ) REPRESENTATION_RELATIONSHIP_WITH_TRANSFORMATION ( #20418 )SHAPE_REPRESENTATION_RELATIONSHIP( ) );
#20885 = CIRCLE ( 'NONE', #14263, 2.500000000000002220 ) ;
#20884 = CARTESIAN_POINT ( 'NONE',  ( 42.50000000000000000, 10.00000000000000000, 44.99999999999999289 ) ) ;
#20886 = CARTESIAN_POINT ( 'NONE',  ( 5.651049729919324527, 39.99999999999999289, 51.93203805547999963 ) ) ;
#20887 = CARTESIAN_POINT ( 'NONE',  ( -7.902600844548947734, 39.58333017843621349, -53.79900150422385252 ) ) ;
#20888 = ORIENTED_EDGE ( 'NONE', *, *, #7442, .T. ) ;
#20889 = CARTESIAN_POINT ( 'NONE',  ( -42.50000000000000711, -12.00000000000000000, 54.00000000000000711 ) ) ;
#20890 = LINE ( 'NONE', #8735, #20658 ) ;
#20891 = ORIENTED_EDGE ( 'NONE', *, *, #748, .T. ) ;
#20892 = DIRECTION ( 'NONE',  ( -1.067522139062650671E-15, 0.000000000000000000, -1.000000000000000000 ) ) ;
#20893 = EDGE_CURVE ( 'NONE', #12579, #1894, #11210, .T. ) ;
#20894 = CARTESIAN_POINT ( 'NONE',  ( 12.99999999999999467, 20.00000000000000000, 11.32475165290614960 ) ) ;
#20895 = CARTESIAN_POINT ( 'NONE',  ( -42.50000000000000711, -5.000000000000000000, -47.50000000000000000 ) ) ;
#20896 = FACE_OUTER_BOUND ( 'NONE', #1177, .T. ) ;
#20897 = ORIENTED_EDGE ( 'NONE', *, *, #2829, .T. ) ;
#20898 = VECTOR ( 'NONE', #7134, 1000.000000000000114 ) ;
#20899 = ORIENTED_EDGE ( 'NONE', *, *, #10998, .F. ) ;
#20900 = ORIENTED_EDGE ( 'NONE', *, *, #12534, .F. ) ;
#20901 = ORIENTED_EDGE ( 'NONE', *, *, #17504, .T. ) ;
#20902 = DIRECTION ( 'NONE',  ( 6.505213034913038160E-19, 3.903127820947822896E-18, 1.000000000000000000 ) ) ;
#20903 = CARTESIAN_POINT ( 'NONE',  ( 22.16820537380700173, 16.50892643625843448, 58.61209530626889830 ) ) ;
#20904 = FACE_OUTER_BOUND ( 'NONE', #20110, .T. ) ;
#20905 = CARTESIAN_POINT ( 'NONE',  ( 4.794048089945632363, 40.00000000000000000, 51.50619359082698878 ) ) ;
#20906 = ORIENTED_EDGE ( 'NONE', *, *, #519, .F. ) ;
#20907 = CARTESIAN_POINT ( 'NONE',  ( 32.83234229683740324, -11.85401191286897316, 2.999999999999995559 ) ) ;
#20908 = DIRECTION ( 'NONE',  ( -6.505213034913038160E-19, -3.903127820947822896E-18, -1.000000000000000000 ) ) ;
#20909 = ORIENTED_EDGE ( 'NONE', *, *, #1333, .T. ) ;
#20910 = EDGE_CURVE ( 'NONE', #6172, #862, #17444, .T. ) ;
#20911 = CARTESIAN_POINT ( 'NONE',  ( -2.516035484449607118, 0.1456407669953184991, 52.33281532376254575 ) ) ;
#20912 = DIRECTION ( 'NONE',  ( 0.000000000000000000, -1.000000000000000000, 0.000000000000000000 ) ) ;
#20913 = ORIENTED_EDGE ( 'NONE', *, *, #13426, .F. ) ;
#20914 = CARTESIAN_POINT ( 'NONE',  ( 1.110223024625156540E-13, -5.551115123125782702E-14, -6.999999999999950262 ) ) ;
#20915 = EDGE_LOOP ( 'NONE', ( #12316, #21714, #22286 ) ) ;
#20916 = CARTESIAN_POINT ( 'NONE',  ( 7.704853968945537979, 39.66343356457746694, -53.66055573870352191 ) ) ;
#20917 = CARTESIAN_POINT ( 'NONE',  ( -7.928368521050097151, 38.36676511147829416, 56.15748794203494754 ) ) ;
#20918 = CARTESIAN_POINT ( 'NONE',  ( -0.5472028025208371949, 39.99822772478366062, 49.15514354140995579 ) ) ;
#20919 = EDGE_CURVE ( 'NONE', #22397, #9047, #19655, .T. ) ;
#20920 = CARTESIAN_POINT ( 'NONE',  ( 2.775557561562891351E-14, -2.775557561562891351E-14, 2.999999999999999112 ) ) ;
#20921 = DIRECTION ( 'NONE',  ( -6.505213034913038160E-19, -3.903127820947822896E-18, -1.000000000000000000 ) ) ;
#20922 = CARTESIAN_POINT ( 'NONE',  ( 29.33526866242106124, -22.15900668633785742, 2.800654218530492123 ) ) ;
#20923 = EDGE_LOOP ( 'NONE', ( #11926, #16369, #9989, #568 ) ) ;
#20924 = AXIS2_PLACEMENT_3D ( 'NONE', #7130, #15824, #21120 ) ;
#20925 = EDGE_LOOP ( 'NONE', ( #15693, #16568, #19961 ) ) ;
#20926 = EDGE_CURVE ( 'NONE', #8398, #19833, #16503, .T. ) ;
#20927 = ORIENTED_EDGE ( 'NONE', *, *, #12226, .T. ) ;
#20928 = ORIENTED_EDGE ( 'NONE', *, *, #17140, .F. ) ;
#20929 = FACE_OUTER_BOUND ( 'NONE', #13095, .T. ) ;
#20930 = CARTESIAN_POINT ( 'NONE',  ( 42.50000000000000711, -5.000000000000000000, 45.40000000000001279 ) ) ;
#20931 = CARTESIAN_POINT ( 'NONE',  ( -11.87329829275383375, 39.99999999999997868, -54.28004929202754170 ) ) ;
#20932 = DIRECTION ( 'NONE',  ( 6.505213034913038160E-19, 3.903127820947822896E-18, 1.000000000000000000 ) ) ;
#20933 = CARTESIAN_POINT ( 'NONE',  ( 0.1155398381881750092, 39.99992209574985225, 48.82370845058371600 ) ) ;
#20934 = ADVANCED_FACE ( 'NONE', ( #16271 ), #6081, .T. ) ;
#20935 = ADVANCED_FACE ( 'NONE', ( #21903 ), #8672, .F. ) ;
#20936 = EDGE_LOOP ( 'NONE', ( #11160, #22121, #9324, #13143 ) ) ;
#20937 = DIRECTION ( 'NONE',  ( 0.000000000000000000, -1.000000000000000000, 0.000000000000000000 ) ) ;
#20938 = FACE_OUTER_BOUND ( 'NONE', #2346, .T. ) ;
#20939 = DIRECTION ( 'NONE',  ( -1.000000000000000000, 0.000000000000000000, 0.000000000000000000 ) ) ;
#20940 = CARTESIAN_POINT ( 'NONE',  ( 89.99999999999701572, -5.000000000000000000, -5.216535399428728743E-14 ) ) ;
#20941 = CARTESIAN_POINT ( 'NONE',  ( -23.50000000000001066, 19.99999999999982947, -105.0010000000000048 ) ) ;
#20942 = ORIENTED_EDGE ( 'NONE', *, *, #17725, .T. ) ;
#20943 =( NAMED_UNIT ( * ) PLANE_ANGLE_UNIT ( ) SI_UNIT ( $, .RADIAN. ) );
#20944 = CARTESIAN_POINT ( 'NONE',  ( 42.50000000000000711, -12.00000000000000000, -47.50000000000000000 ) ) ;
#20945 = CARTESIAN_POINT ( 'NONE',  ( 2.775557561562891351E-14, -2.775557561562891351E-14, 2.999999999999999112 ) ) ;
#20946 = DIRECTION ( 'NONE',  ( 0.000000000000000000, 0.000000000000000000, 1.000000000000000000 ) ) ;
#20947 = DIRECTION ( 'NONE',  ( 0.000000000000000000, -1.000000000000000000, 0.000000000000000000 ) ) ;
#20948 = ORIENTED_EDGE ( 'NONE', *, *, #163, .F. ) ;
#20949 = VERTEX_POINT ( 'NONE', #9176 ) ;
#20950 = ADVANCED_FACE ( 'NONE', ( #21438 ), #18550, .F. ) ;
#20951 = ORIENTED_EDGE ( 'NONE', *, *, #10822, .T. ) ;
#20952 = CARTESIAN_POINT ( 'NONE',  ( -14.29266125237879592, 28.07080038625078799, -7.000000000000006217 ) ) ;
#20953 = DIRECTION ( 'NONE',  ( -0.000000000000000000, -1.000000000000000000, -0.000000000000000000 ) ) ;
#20954 = EDGE_CURVE ( 'NONE', #1383, #3928, #7574, .T. ) ;
#20955 = ADVANCED_FACE ( 'NONE', ( #2422 ), #10846, .T. ) ;
#20956 = ORIENTED_EDGE ( 'NONE', *, *, #16173, .F. ) ;
#20957 = B_SPLINE_CURVE_WITH_KNOTS ( 'NONE', 3,
 ( #19582, #554, #21531, #19472, #7547, #17861, #2167, #12245, #12358, #7093, #3892, #10625, #15786, #8920, #19253, #21077, #21189, #5381, #12459, #10859, #19370, #17630 ),
 .UNSPECIFIED., .F., .F.,
 ( 4, 2, 2, 2, 2, 2, 2, 2, 2, 2, 4 ),
 ( 0.007712149587921488143, 0.01231940472852635984, 0.01347121851367757625, 0.01462303229882878919, 0.01692665986913123241, 0.01807847365428245229, 0.01923028743943366869, 0.02153391500973611192, 0.02268572879488733526, 0.02383754258003855514, 0.02614117015034099489 ),
 .UNSPECIFIED. ) ;
#20958 = CARTESIAN_POINT ( 'NONE',  ( 2.775557561562891351E-14, 2.775557561562891351E-14, 5.750000000000001776 ) ) ;
#20959 = CYLINDRICAL_SURFACE ( 'NONE', #19855, 0.9999999999999991118 ) ;
#20960 = DIRECTION ( 'NONE',  ( -1.000000000000000000, 0.000000000000000000, 0.000000000000000000 ) ) ;
#20961 = CARTESIAN_POINT ( 'NONE',  ( -18.88991738967393275, 26.58741517404049048, -57.84428223557713267 ) ) ;
#20962 = EDGE_CURVE ( 'NONE', #11090, #13123, #14550, .T. ) ;
#20963 = DIRECTION ( 'NONE',  ( 0.000000000000000000, 0.000000000000000000, 1.000000000000000000 ) ) ;
#20964 = ORIENTED_EDGE ( 'NONE', *, *, #14597, .F. ) ;
#20965 = DIRECTION ( 'NONE',  ( 6.505213034913038160E-19, 3.903127820947822896E-18, 1.000000000000000000 ) ) ;
#20966 = CARTESIAN_POINT ( 'NONE',  ( 35.00000000000001421, -5.000000000000000000, 4.999999999999997335 ) ) ;
#20967 = ADVANCED_FACE ( 'NONE', ( #16149 ), #5860, .T. ) ;
#20968 = CARTESIAN_POINT ( 'NONE',  ( -35.16985127952374057, -10.70799354677395776, -2.800654218530457484 ) ) ;
#20969 = CARTESIAN_POINT ( 'NONE',  ( 3.608224830031758756E-13, -2.775557561562891351E-14, -4.999999999999997335 ) ) ;
#20970 = EDGE_LOOP ( 'NONE', ( #7891, #14360, #5997, #4391 ) ) ;
#20971 = CARTESIAN_POINT ( 'NONE',  ( -26.79308242454895961, -16.56444186175090749, 2.999999999999995559 ) ) ;
#20972 = CONICAL_SURFACE ( 'NONE', #9610, 2.099999999999997868, 1.029744258676652091 ) ;
#20973 = ORIENTED_EDGE ( 'NONE', *, *, #13080, .F. ) ;
#20974 = ITEM_DEFINED_TRANSFORMATION ( 'NONE', 'NONE', #14209,  #18273 ) ;
#20975 = EDGE_LOOP ( 'NONE', ( #5514, #21442, #21449, #16401 ) ) ;
#20976 = CARTESIAN_POINT ( 'NONE',  ( -42.50000000000000711, -11.97499999999999964, 47.50000000000000711 ) ) ;
#20977 = CYLINDRICAL_SURFACE ( 'NONE', #21601, 2.500000000000008882 ) ;
#20978 = AXIS2_PLACEMENT_3D ( 'NONE', #21374, #9344, #5671 ) ;
#20979 = LINE ( 'NONE', #21201, #20774 ) ;
#20980 = LINE ( 'NONE', #20756, #18630 ) ;
#20981 = ORIENTED_EDGE ( 'NONE', *, *, #13765, .F. ) ;
#20982 = LINE ( 'NONE', #10086, #16048 ) ;
#20983 = AXIS2_PLACEMENT_3D ( 'NONE', #2459, #739, #7720 ) ;
#20984 = CARTESIAN_POINT ( 'NONE',  ( -11.09836907989745569, 40.00000000000000000, -54.00358115607139808 ) ) ;
#20985 = VERTEX_POINT ( 'NONE', #704 ) ;
#20986 = CARTESIAN_POINT ( 'NONE',  ( 6.699391982050356020, -4.821764332415713561, -49.69317737456918849 ) ) ;
#20987 = AXIS2_PLACEMENT_3D ( 'NONE', #2921, #2802, #9896 ) ;
#20988 = EDGE_CURVE ( 'NONE', #3268, #15217, #22287, .T. ) ;
#20989 = CARTESIAN_POINT ( 'NONE',  ( 15.67632863000011056, 36.06985656533340290, -56.80410608597895816 ) ) ;
#20990 = DIRECTION ( 'NONE',  ( 0.7071067811865463515, 0.000000000000000000, 0.7071067811865487940 ) ) ;
#20991 = EDGE_CURVE ( 'NONE', #4363, #10740, #6108, .T. ) ;
#20992 = DIRECTION ( 'NONE',  ( -1.000000000000000000, 0.000000000000000000, 0.000000000000000000 ) ) ;
#20993 = CARTESIAN_POINT ( 'NONE',  ( 9.855264211176361755, 31.32970427768389499, -43.22210574525156801 ) ) ;
#20994 = EDGE_LOOP ( 'NONE', ( #21243, #4642, #7186, #16990, #10454 ) ) ;
#20995 = CARTESIAN_POINT ( 'NONE',  ( -35.00000000000000000, -4.999999999999997335, 1.387778780781445676E-14 ) ) ;
#20996 = CARTESIAN_POINT ( 'NONE',  ( -19.90072640592962117, 9.610007367499633801, 58.06946678856481725 ) ) ;
#20997 = ORIENTED_EDGE ( 'NONE', *, *, #14947, .T. ) ;
#20998 = AXIS2_PLACEMENT_3D ( 'NONE', #21611, #3975, #21844 ) ;
#20999 = EDGE_CURVE ( 'NONE', #22470, #12493, #4041, .T. ) ;
#21000 = DIRECTION ( 'NONE',  ( 6.505213034913038160E-19, 3.903127820947822896E-18, 1.000000000000000000 ) ) ;
#21001 = CARTESIAN_POINT ( 'NONE',  ( 2.602085213965210642E-15, 5.025303850726727362, 0.000000000000000000 ) ) ;
#21002 = PRODUCT_DEFINITION_SHAPE ( 'NONE', 'NONE',  #20341 ) ;
#21003 = AXIS2_PLACEMENT_3D ( 'NONE', #7736, #15978, #17701 ) ;
#21004 = AXIS2_PLACEMENT_3D ( 'NONE', #2541, #9524, #15445 ) ;
#21005 = CIRCLE ( 'NONE', #8549, 2.499999999999995115 ) ;
#21006 = ORIENTED_EDGE ( 'NONE', *, *, #17290, .F. ) ;
#21007 = ORIENTED_EDGE ( 'NONE', *, *, #6240, .T. ) ;
#21008 = ORIENTED_EDGE ( 'NONE', *, *, #12523, .F. ) ;
#21009 = SHAPE_REPRESENTATION_RELATIONSHIP ( 'NONE' , 'NONE' ,  #21292, #7741 ) ;
#21010 = VERTEX_POINT ( 'NONE', #17994 ) ;
#21011 = CYLINDRICAL_SURFACE ( 'NONE', #6319, 19.11328065563150957 ) ;
#21012 = CARTESIAN_POINT ( 'NONE',  ( 13.32368996328068356, 38.03919112700259575, 55.94897837928601803 ) ) ;
#21013 = EDGE_CURVE ( 'NONE', #11834, #5053, #2300, .T. ) ;
#21014 = CIRCLE ( 'NONE', #12219, 31.50000000000001421 ) ;
#21015 = DIRECTION ( 'NONE',  ( 0.000000000000000000, 0.000000000000000000, -1.000000000000000000 ) ) ;
#21016 = EDGE_LOOP ( 'NONE', ( #2799, #9215, #7557, #10241, #2110, #399 ) ) ;
#21017 = CARTESIAN_POINT ( 'NONE',  ( -35.00000000000000000, -9.000000000000001776, 1.387778780781445676E-14 ) ) ;
#21018 = CARTESIAN_POINT ( 'NONE',  ( 0.6864184775310656628, -1.216838870810526219, -47.75834167803935060 ) ) ;
#21019 = VERTEX_POINT ( 'NONE', #7571 ) ;
#21020 = FACE_OUTER_BOUND ( 'NONE', #10958, .T. ) ;
#21021 = AXIS2_PLACEMENT_3D ( 'NONE', #2524, #6062, #7900 ) ;
#21022 = ORIENTED_EDGE ( 'NONE', *, *, #6271, .T. ) ;
#21023 = DIRECTION ( 'NONE',  ( 6.505213034913038160E-19, 3.903127820947822896E-18, 1.000000000000000000 ) ) ;
#21024 = VERTEX_POINT ( 'NONE', #19840 ) ;
#21025 = DIRECTION ( 'NONE',  ( -1.000000000000000000, -1.208970125616060101E-17, 6.505213034913038160E-19 ) ) ;
#21026 = CARTESIAN_POINT ( 'NONE',  ( 4.718447854656915297E-13, -22.00000000000021316, -2.999999999999971578 ) ) ;
#21027 = DIRECTION ( 'NONE',  ( -6.505213034913038160E-19, -3.903127820947822896E-18, -1.000000000000000000 ) ) ;
#21028 = AXIS2_PLACEMENT_3D ( 'NONE', #6876, #19131, #17281 ) ;
#21029 = CARTESIAN_POINT ( 'NONE',  ( 18.82278182890044604, 26.77493817624154460, 60.32982055024199752 ) ) ;
#21030 = DIRECTION ( 'NONE',  ( 1.000000000000000000, 0.000000000000000000, 0.000000000000000000 ) ) ;
#21031 = DIRECTION ( 'NONE',  ( -0.000000000000000000, 1.000000000000000000, -0.000000000000000000 ) ) ;
#21033 = EDGE_LOOP ( 'NONE', ( #3021, #1694 ) ) ;
#21032 = EDGE_CURVE ( 'NONE', #7317, #20449, #12136, .T. ) ;
#21034 = AXIS2_PLACEMENT_3D ( 'NONE', #20272, #8123, #18546 ) ;
#21035 = ORIENTED_EDGE ( 'NONE', *, *, #1103, .F. ) ;
#21036 = ORIENTED_EDGE ( 'NONE', *, *, #5361, .F. ) ;
#21037 = VERTEX_POINT ( 'NONE', #8030 ) ;
#21038 = FACE_OUTER_BOUND ( 'NONE', #6834, .T. ) ;
#21039 = EDGE_CURVE ( 'NONE', #16276, #3830, #16715, .T. ) ;
#21040 = FACE_OUTER_BOUND ( 'NONE', #12214, .T. ) ;
#21041 = FACE_OUTER_BOUND ( 'NONE', #4459, .T. ) ;
#21042 = CARTESIAN_POINT ( 'NONE',  ( 2.213007027836657148, 39.97050984159520226, 50.37695261049397288 ) ) ;
#21043 = VERTEX_POINT ( 'NONE', #6536 ) ;
#21044 = DIRECTION ( 'NONE',  ( 0.000000000000000000, 0.000000000000000000, 1.000000000000000000 ) ) ;
#21045 = CARTESIAN_POINT ( 'NONE',  ( 28.06260833510307151, -14.30873905802340573, -2.999999999999971578 ) ) ;
#21046 = CARTESIAN_POINT ( 'NONE',  ( 28.49999999999998224, 19.99999999999999645, -100.0000000000000000 ) ) ;
#21047 = DIRECTION ( 'NONE',  ( -0.000000000000000000, -1.000000000000000000, -0.000000000000000000 ) ) ;
#21048 = FILL_AREA_STYLE_COLOUR ( '', #2169 ) ;
#21049 = AXIS2_PLACEMENT_3D ( 'NONE', #3242, #11712, #6447 ) ;
#21050 = ADVANCED_FACE ( 'NONE', ( #4713 ), #9859, .F. ) ;
#21051 = FILL_AREA_STYLE ('',( #1811 ) ) ;
#21052 = PLANE ( 'NONE',  #1021 ) ;
#21053 = CARTESIAN_POINT ( 'NONE',  ( -7.704858207814790916, 39.66343987625801759, 53.66055254569381106 ) ) ;
#21054 = DIRECTION ( 'NONE',  ( -0.000000000000000000, 1.000000000000000000, -0.000000000000000000 ) ) ;
#21055 = CARTESIAN_POINT ( 'NONE',  ( 35.00000000000000000, 0.000000000000000000, 41.00000000000002132 ) ) ;
#21056 = VECTOR ( 'NONE', #18610, 1000.000000000000000 ) ;
#21057 = EDGE_CURVE ( 'NONE', #9968, #20345, #17812, .T. ) ;
#21058 = ORIENTED_EDGE ( 'NONE', *, *, #7240, .F. ) ;
#21059 = VECTOR ( 'NONE', #22581, 1000.000000000000000 ) ;
#21060 = EDGE_LOOP ( 'NONE', ( #5674, #1236, #7305, #20579 ) ) ;
#21061 = EDGE_LOOP ( 'NONE', ( #20956, #21670, #7410, #21526 ) ) ;
#21062 = CIRCLE ( 'NONE', #4235, 5.000000000000000000 ) ;
#21063 = CARTESIAN_POINT ( 'NONE',  ( -1.387778780781445676E-14, 20.00000000000000000, -101.0000000000000284 ) ) ;
#21064 = DIRECTION ( 'NONE',  ( -6.505213034913038160E-19, -3.903127820947822896E-18, -1.000000000000000000 ) ) ;
#21065 = CARTESIAN_POINT ( 'NONE',  ( -90.00000000000000000, 28.00000000000000000, -9.108981535246192915E-16 ) ) ;
#21066 = CARTESIAN_POINT ( 'NONE',  ( -18.48876241336181536, 12.20729522219679986, 60.24712676880315598 ) ) ;
#21067 = CIRCLE ( 'NONE', #7157, 59.99999999999700862 ) ;
#21068 = CARTESIAN_POINT ( 'NONE',  ( -11.24237306623856014, 36.54654314592846021, -57.72256821685509465 ) ) ;
#21069 = VECTOR ( 'NONE', #17005, 1000.000000000000000 ) ;
#21070 = FACE_BOUND ( 'NONE', #242, .T. ) ;
#21071 = VECTOR ( 'NONE', #19890, 1000.000000000000000 ) ;
#21072 = ADVANCED_FACE ( 'NONE', ( #16728 ), #10489, .T. ) ;
#21073 = ORIENTED_EDGE ( 'NONE', *, *, #13793, .T. ) ;
#21074 = CARTESIAN_POINT ( 'NONE',  ( 12.00000000000000355, 1.500000000000003553, 0.000000000000000000 ) ) ;
#21075 = CIRCLE ( 'NONE', #15198, 60.00000000000000000 ) ;
#21076 = LINE ( 'NONE', #209, #5356 ) ;
#21077 = CARTESIAN_POINT ( 'NONE',  ( 14.40375226887234561, 15.79546342576959184, -45.56106839101555295 ) ) ;
#21078 = CONICAL_SURFACE ( 'NONE', #2803, 33.99999999999999289, 1.308996938995745873 ) ;
#21079 = VERTEX_POINT ( 'NONE', #3214 ) ;
#21080 = DIRECTION ( 'NONE',  ( 6.505213034913038160E-19, 3.903127820947822896E-18, 1.000000000000000000 ) ) ;
#21081 = DIRECTION ( 'NONE',  ( 3.063596499322173499E-16, 0.000000000000000000, -1.000000000000000000 ) ) ;
#21082 = EDGE_CURVE ( 'NONE', #18681, #16159, #20747, .T. ) ;
#21083 = EDGE_CURVE ( 'NONE', #15608, #8384, #1146, .T. ) ;
#21084 = AXIS2_PLACEMENT_3D ( 'NONE', #9025, #2158, #9247 ) ;
#21085 = AXIS2_PLACEMENT_3D ( 'NONE', #5702, #17849, #9027 ) ;
#21086 = ORIENTED_EDGE ( 'NONE', *, *, #11406, .F. ) ;
#21087 = CIRCLE ( 'NONE', #7554, 10.00000000000000178 ) ;
#21088 = AXIS2_PLACEMENT_3D ( 'NONE', #12458, #2048, #10400 ) ;
#21089 = EDGE_CURVE ( 'NONE', #8364, #14167, #13262, .T. ) ;
#21090 = VERTEX_POINT ( 'NONE', #20291 ) ;
#21091 = DIRECTION ( 'NONE',  ( -0.000000000000000000, 1.000000000000000000, -0.000000000000000000 ) ) ;
#21092 = EDGE_CURVE ( 'NONE', #5279, #2407, #9413, .T. ) ;
#21093 = CARTESIAN_POINT ( 'NONE',  ( -13.06969024216335740, -19.15111107797470780, -2.999999999999995559 ) ) ;
#21094 = CARTESIAN_POINT ( 'NONE',  ( -34.99999999999980815, 40.00000000000000711, 54.99999999999922551 ) ) ;
#21095 = CARTESIAN_POINT ( 'NONE',  ( -1.387778780781445518E-14, 20.00000000000000355, 103.0000000000000284 ) ) ;
#21096 = ORIENTED_EDGE ( 'NONE', *, *, #17859, .T. ) ;
#21097 = FACE_BOUND ( 'NONE', #22055, .T. ) ;
#21098 = DIRECTION ( 'NONE',  ( 6.505213034913038160E-19, 3.903127820947822896E-18, 1.000000000000000000 ) ) ;
#21099 = EDGE_LOOP ( 'NONE', ( #2275, #15999, #17231, #9366 ) ) ;
#21100 = DIRECTION ( 'NONE',  ( 0.000000000000000000, 0.000000000000000000, 1.000000000000000000 ) ) ;
#21101 = CARTESIAN_POINT ( 'NONE',  ( -7.882609639814679786E-15, -9.552912840896525389E-26, -50.50395615645409464 ) ) ;
#21102 = CYLINDRICAL_SURFACE ( 'NONE', #18492, 22.00000000000000711 ) ;
#21103 = CARTESIAN_POINT ( 'NONE',  ( -1.387778780781445676E-14, 20.00000000000000000, 60.00200000000000244 ) ) ;
#21104 = VERTEX_POINT ( 'NONE', #18682 ) ;
#21105 = DIRECTION ( 'NONE',  ( -1.000000000000000000, 0.000000000000000000, 0.000000000000000000 ) ) ;
#21106 = CARTESIAN_POINT ( 'NONE',  ( -2.665760015255949078, 39.95807811140273458, -50.69599157361079023 ) ) ;
#21107 = VECTOR ( 'NONE', #583, 1000.000000000000000 ) ;
#21108 = EDGE_LOOP ( 'NONE', ( #3574, #12455, #21096, #9719 ) ) ;
#21109 = DIRECTION ( 'NONE',  ( -1.000000000000000000, -1.208970125616083212E-17, 0.000000000000000000 ) ) ;
#21110 = LINE ( 'NONE', #2197, #19509 ) ;
#21111 = AXIS2_PLACEMENT_3D ( 'NONE', #15995, #19455, #7182 ) ;
#21113 = EDGE_CURVE ( 'NONE', #13475, #19379, #1344, .T. ) ;
#21112 = EDGE_LOOP ( 'NONE', ( #19459, #16754, #15410, #4154 ) ) ;
#21114 = ADVANCED_FACE ( 'NONE', ( #8365 ), #6417, .F. ) ;
#21115 = VERTEX_POINT ( 'NONE', #15679 ) ;
#21116 = CIRCLE ( 'NONE', #996, 20.00000000000000000 ) ;
#21117 = ORIENTED_EDGE ( 'NONE', *, *, #21966, .F. ) ;
#21118 = VECTOR ( 'NONE', #19248, 1000.000000000000000 ) ;
#21119 = VERTEX_POINT ( 'NONE', #3773 ) ;
#21120 = DIRECTION ( 'NONE',  ( 0.000000000000000000, 0.000000000000000000, -1.000000000000000000 ) ) ;
#21121 = CARTESIAN_POINT ( 'NONE',  ( 21.99996130922171389, 24.71724789032312586, 58.57718774367118186 ) ) ;
#21122 = CARTESIAN_POINT ( 'NONE',  ( 4.171001175319766219, 35.79662727779869869, 3.000000000000009770 ) ) ;
#21123 = CARTESIAN_POINT ( 'NONE',  ( 4.465627656007536750, 40.00000000000000000, 51.33835359896442441 ) ) ;
#21124 = ADVANCED_FACE ( 'NONE', ( #17737 ), #17397, .T. ) ;
#21125 = ORIENTED_EDGE ( 'NONE', *, *, #21309, .T. ) ;
#21126 = DIRECTION ( 'NONE',  ( -1.000000000000000000, 0.000000000000000000, -0.000000000000000000 ) ) ;
#21127 = CARTESIAN_POINT ( 'NONE',  ( 22.12933039895922249, 28.19616000222403329, 2.710061364035962525E-15 ) ) ;
#21128 = ORIENTED_EDGE ( 'NONE', *, *, #10191, .F. ) ;
#21129 = CARTESIAN_POINT ( 'NONE',  ( -35.00000000000000000, 22.00000000000000355, -16.99999999999997868 ) ) ;
#21130 = DIRECTION ( 'NONE',  ( 0.000000000000000000, 0.000000000000000000, -1.000000000000000000 ) ) ;
#21131 = VERTEX_POINT ( 'NONE', #16014 ) ;
#21132 = CARTESIAN_POINT ( 'NONE',  ( 9.103081159015337320, 0.03030367950460435486, 53.87333532811651793 ) ) ;
#21133 = EDGE_LOOP ( 'NONE', ( #5211, #1087, #5131, #21490 ) ) ;
#21134 = CARTESIAN_POINT ( 'NONE',  ( 1.575029502094859701, 39.98856664293944618, -49.93404254833944123 ) ) ;
#21135 = FACE_OUTER_BOUND ( 'NONE', #16583, .T. ) ;
#21136 = CARTESIAN_POINT ( 'NONE',  ( -4.517334468824944160, 39.87309017818895995, 51.91252173886011434 ) ) ;
#21137 = CIRCLE ( 'NONE', #15637, 2.499999999999998668 ) ;
#21138 = ADVANCED_BREP_SHAPE_REPRESENTATION ( '', ( #10617, #18273 ), #22313 ) ;
#21139 = AXIS2_PLACEMENT_3D ( 'NONE', #7226, #14194, #21318 ) ;
#21140 = CARTESIAN_POINT ( 'NONE',  ( 19.81381843823947264, 22.85613052104596932, 58.09821304537223341 ) ) ;
#21141 = DIRECTION ( 'NONE',  ( -0.000000000000000000, 1.000000000000000000, -0.000000000000000000 ) ) ;
#21142 = AXIS2_PLACEMENT_3D ( 'NONE', #659, #7756, #14956 ) ;
#21143 = DIRECTION ( 'NONE',  ( -1.000000000000000000, 0.000000000000000000, 0.000000000000000000 ) ) ;
#21144 = ORIENTED_EDGE ( 'NONE', *, *, #12206, .F. ) ;
#21145 = CIRCLE ( 'NONE', #1771, 58.99999999999994316 ) ;
#21146 = ORIENTED_EDGE ( 'NONE', *, *, #18187, .F. ) ;
#21147 = ORIENTED_EDGE ( 'NONE', *, *, #18719, .F. ) ;
#21148 = DIRECTION ( 'NONE',  ( 0.000000000000000000, 0.000000000000000000, 1.000000000000000000 ) ) ;
#21149 = PLANE ( 'NONE',  #1937 ) ;
#21150 = AXIS2_PLACEMENT_3D ( 'NONE', #15435, #11780, #20960 ) ;
#21151 = AXIS2_PLACEMENT_3D ( 'NONE', #7519, #14939, #5802 ) ;
#21152 = CARTESIAN_POINT ( 'NONE',  ( 42.50000000000000711, -5.000000000000000000, 47.50000000000000711 ) ) ;
#21153 = DIRECTION ( 'NONE',  ( -0.000000000000000000, 1.000000000000000000, -0.000000000000000000 ) ) ;
#21154 = CARTESIAN_POINT ( 'NONE',  ( 1.103251425233469529, 39.99275656736713813, 49.57314630728770766 ) ) ;
#21155 = AXIS2_PLACEMENT_3D ( 'NONE', #3404, #15980, #11133 ) ;
#21156 = ORIENTED_EDGE ( 'NONE', *, *, #13711, .T. ) ;
#21157 = LINE ( 'NONE', #18387, #7903 ) ;
#21158 = DIRECTION ( 'NONE',  ( 0.000000000000000000, 0.000000000000000000, -1.000000000000000000 ) ) ;
#21159 = CARTESIAN_POINT ( 'NONE',  ( 35.00000000000000000, 17.00000000000000000, 39.00000000000003553 ) ) ;
#21160 = DIRECTION ( 'NONE',  ( -0.000000000000000000, 1.000000000000000000, -0.000000000000000000 ) ) ;
#21161 = B_SPLINE_CURVE_WITH_KNOTS ( 'NONE', 3,
 ( #1988, #44, #10458, #15953, #21347, #13991, #14339, #262 ),
 .UNSPECIFIED., .F., .F.,
 ( 4, 2, 2, 4 ),
 ( 0.001329099847188741938, 0.002445656686148434990, 0.003562213525108127825, 0.005795327203027498750 ),
 .UNSPECIFIED. ) ;
#21162 =( NAMED_UNIT ( * ) PLANE_ANGLE_UNIT ( ) SI_UNIT ( $, .RADIAN. ) );
#21163 = ADVANCED_FACE ( 'NONE', ( #12135 ), #205, .T. ) ;
#21164 = AXIS2_PLACEMENT_3D ( 'NONE', #2276, #9262, #9603 ) ;
#21165 = DIRECTION ( 'NONE',  ( -6.505213034913038160E-19, -3.903127820947822896E-18, -1.000000000000000000 ) ) ;
#21166 = CIRCLE ( 'NONE', #19700, 25.00000000000000711 ) ;
#21167 = ADVANCED_FACE ( 'NONE', ( #7199 ), #14168, .T. ) ;
#21168 = DIRECTION ( 'NONE',  ( -6.505213034913038160E-19, -3.903127820947822896E-18, -1.000000000000000000 ) ) ;
#21169 = CARTESIAN_POINT ( 'NONE',  ( -31.47514467962681550, 17.79500259159609499, 2.932460736555816627 ) ) ;
#21170 = AXIS2_PLACEMENT_3D ( 'NONE', #3279, #16796, #1202 ) ;
#21171 = FACE_OUTER_BOUND ( 'NONE', #13741, .T. ) ;
#21172 = CIRCLE ( 'NONE', #3634, 2.499999999999996891 ) ;
#21173 = ORIENTED_EDGE ( 'NONE', *, *, #15085, .F. ) ;
#21174 = VERTEX_POINT ( 'NONE', #15783 ) ;
#21175 = EDGE_LOOP ( 'NONE', ( #9758, #14082, #14823 ) ) ;
#21176 = CARTESIAN_POINT ( 'NONE',  ( 5.961618526219221614, -3.061744126945400879, -51.29856354178556188 ) ) ;
#21177 = AXIS2_PLACEMENT_3D ( 'NONE', #16921, #5613, #14545 ) ;
#21178 = LINE ( 'NONE', #422, #1373 ) ;
#21179 = CARTESIAN_POINT ( 'NONE',  ( 1.110223024625156540E-13, -24.99999999999999289, 3.000000000000023537 ) ) ;
#21180 = LINE ( 'NONE', #5481, #11192 ) ;
#21181 = DIRECTION ( 'NONE',  ( -1.000000000000000000, 8.702939542935596068E-14, 0.000000000000000000 ) ) ;
#21182 = EDGE_CURVE ( 'NONE', #2480, #7279, #14123, .T. ) ;
#21183 = DIRECTION ( 'NONE',  ( 1.000000000000000000, 0.000000000000000000, -1.445602896647339163E-16 ) ) ;
#21184 = CARTESIAN_POINT ( 'NONE',  ( -14.94062893683336668, 21.54390686295444368, -45.79998742252194432 ) ) ;
#21185 = ORIENTED_EDGE ( 'NONE', *, *, #590, .T. ) ;
#21186 = CARTESIAN_POINT ( 'NONE',  ( -26.00000000000001421, 19.99999999999982947, 105.0000000000000142 ) ) ;
#21187 = CARTESIAN_POINT ( 'NONE',  ( -8.331955809010631597, 38.18181818181817988, -56.36098470834072316 ) ) ;
#21188 = CARTESIAN_POINT ( 'NONE',  ( -28.50000000000001421, 19.99999999999982947, -105.0010000000000048 ) ) ;
#21189 = CARTESIAN_POINT ( 'NONE',  ( 14.50678847729822252, 16.16560534949679351, -45.60743157421818950 ) ) ;
#21190 = ADVANCED_FACE ( 'NONE', ( #17280 ), #16351, .T. ) ;
#21191 = VERTEX_POINT ( 'NONE', #13943 ) ;
#21192 = DIRECTION ( 'NONE',  ( -1.000000000000000000, 1.234337511092497482E-14, 0.000000000000000000 ) ) ;
#21193 = FACE_OUTER_BOUND ( 'NONE', #7399, .T. ) ;
#21194 = AXIS2_PLACEMENT_3D ( 'NONE', #5987, #16524, #9541 ) ;
#21195 = ORIENTED_EDGE ( 'NONE', *, *, #3394, .T. ) ;
#21196 = ADVANCED_FACE ( 'NONE', ( #14051 ), #6874, .T. ) ;
#21197 = ITEM_DEFINED_TRANSFORMATION ( 'NONE', 'NONE', #11302,  #18273 ) ;
#21198 = VERTEX_POINT ( 'NONE', #10515 ) ;
#21199 = CARTESIAN_POINT ( 'NONE',  ( 3.460816278822046447E-15, -1.500000000000015099, 0.000000000000000000 ) ) ;
#21200 = DIRECTION ( 'NONE',  ( -6.505213034913038160E-19, -3.903127820947822896E-18, -1.000000000000000000 ) ) ;
#21201 = CARTESIAN_POINT ( 'NONE',  ( -11.35354668330680639, -30.33632613426187774, -7.000000000000006217 ) ) ;
#21202 = AXIS2_PLACEMENT_3D ( 'NONE', #21529, #9498, #18309 ) ;
#21203 = CARTESIAN_POINT ( 'NONE',  ( -42.49999999999996447, 10.00000000000000000, -45.00000000000000711 ) ) ;
#21204 = ORIENTED_EDGE ( 'NONE', *, *, #20725, .T. ) ;
#21205 = CARTESIAN_POINT ( 'NONE',  ( 2.220446049250313081E-13, -2.498001805406602216E-13, -6.859353255829918616 ) ) ;
#21206 = CARTESIAN_POINT ( 'NONE',  ( -8.732260780949433254, 39.99999999999998579, 53.24192688670174789 ) ) ;
#21207 = ORIENTED_EDGE ( 'NONE', *, *, #7575, .F. ) ;
#21208 = EDGE_CURVE ( 'NONE', #6233, #7580, #5267, .T. ) ;
#21210 = EDGE_CURVE ( 'NONE', #18495, #10435, #6482, .T. ) ;
#21209 = DIRECTION ( 'NONE',  ( -1.000000000000000000, -1.208970125616063644E-17, 0.000000000000000000 ) ) ;
#21211 = DIRECTION ( 'NONE',  ( 0.000000000000000000, 1.000000000000000000, 0.000000000000000000 ) ) ;
#21212 = DIRECTION ( 'NONE',  ( 1.000000000000000000, 0.000000000000000000, 0.000000000000000000 ) ) ;
#21213 = ORIENTED_EDGE ( 'NONE', *, *, #2118, .F. ) ;
#21214 = DIRECTION ( 'NONE',  ( 0.000000000000000000, 0.000000000000000000, 1.000000000000000000 ) ) ;
#21215 = CARTESIAN_POINT ( 'NONE',  ( -9.744263423232602861, 2.495070046656082674, 54.63687069583399136 ) ) ;
#21216 = CARTESIAN_POINT ( 'NONE',  ( -1.092488160344625037, 39.99289796980131229, -49.56515122593324918 ) ) ;
#21217 = ORIENTED_EDGE ( 'NONE', *, *, #12011, .T. ) ;
#21218 = CARTESIAN_POINT ( 'NONE',  ( 89.99999999999701572, -5.000000000000000000, 2.499999999999956479 ) ) ;
#21219 = AXIS2_PLACEMENT_3D ( 'NONE', #20755, #5068, #13616 ) ;
#21220 = LINE ( 'NONE', #8844, #10074 ) ;
#21221 = EDGE_CURVE ( 'NONE', #16362, #21600, #11230, .T. ) ;
#21222 = CARTESIAN_POINT ( 'NONE',  ( -6.696867368503558448E-15, 40.00000000000000000, -48.73397172404479960 ) ) ;
#21223 = CIRCLE ( 'NONE', #12427, 6.499999999999999112 ) ;
#21224 = ADVANCED_FACE ( 'NONE', ( #19469 ), #19022, .F. ) ;
#21225 = EDGE_LOOP ( 'NONE', ( #13795, #13308, #5046, #6396 ) ) ;
#21226 = ORIENTED_EDGE ( 'NONE', *, *, #19224, .F. ) ;
#21227 = ADVANCED_FACE ( 'NONE', ( #1595 ), #8583, .F. ) ;
#21228 = ORIENTED_EDGE ( 'NONE', *, *, #3453, .T. ) ;
#21229 = ORIENTED_EDGE ( 'NONE', *, *, #14262, .F. ) ;
#21230 = CARTESIAN_POINT ( 'NONE',  ( -31.57187188083515750, -7.711478842616581453, -7.000000000000006217 ) ) ;
#21231 = DIRECTION ( 'NONE',  ( -1.000000000000000000, 0.000000000000000000, 0.000000000000000000 ) ) ;
#21232 = CIRCLE ( 'NONE', #14643, 11.00000000000003730 ) ;
#21233 = CARTESIAN_POINT ( 'NONE',  ( 8.553367002852411360, 39.50246935780211999, -54.09836737755986746 ) ) ;
#21234 = CARTESIAN_POINT ( 'NONE',  ( -31.41173278719228179, -17.66631876130928092, 2.999999999999999112 ) ) ;
#21235 = ORIENTED_EDGE ( 'NONE', *, *, #6235, .F. ) ;
#21236 = CARTESIAN_POINT ( 'NONE',  ( -35.33352588067108258, -7.094908322883481055, 2.999999999999999112 ) ) ;
#21237 = DIRECTION ( 'NONE',  ( 1.000000000000000000, 0.000000000000000000, 0.000000000000000000 ) ) ;
#21238 = ORIENTED_EDGE ( 'NONE', *, *, #4426, .F. ) ;
#21239 = EDGE_CURVE ( 'NONE', #20662, #17550, #19367, .T. ) ;
#21240 = DIRECTION ( 'NONE',  ( 6.505213034913038160E-19, 3.903127820947822896E-18, 1.000000000000000000 ) ) ;
#21241 = CARTESIAN_POINT ( 'NONE',  ( 2.602085213965210642E-15, 5.025303850726727362, 0.000000000000000000 ) ) ;
#21242 = CARTESIAN_POINT ( 'NONE',  ( 34.65667543218833657, 4.170748987303380062, 2.999999999999999112 ) ) ;
#21243 = ORIENTED_EDGE ( 'NONE', *, *, #1633, .F. ) ;
#21244 = PLANE ( 'NONE',  #1793 ) ;
#21245 = VERTEX_POINT ( 'NONE', #3670 ) ;
#21246 = CARTESIAN_POINT ( 'NONE',  ( 7.776554266669417956E-15, -4.648749848372173865, -45.43309249825056639 ) ) ;
#21247 = DIRECTION ( 'NONE',  ( -1.000000000000000000, 1.301042606982605814E-16, 0.000000000000000000 ) ) ;
#21248 = CARTESIAN_POINT ( 'NONE',  ( 12.99999999999993960, 42.51666049839543149, -100.0000000000000000 ) ) ;
#21249 = EDGE_CURVE ( 'NONE', #18686, #15823, #10621, .T. ) ;
#21250 = FACE_OUTER_BOUND ( 'NONE', #20975, .T. ) ;
#21251 = DIRECTION ( 'NONE',  ( -6.505213034913038160E-19, -3.903127820947822896E-18, -1.000000000000000000 ) ) ;
#21252 = CARTESIAN_POINT ( 'NONE',  ( 22.42386962120395566, 19.82082524447363525, 58.66720683610022746 ) ) ;
#21253 = EDGE_CURVE ( 'NONE', #18483, #15034, #12329, .T. ) ;
#21254 = CARTESIAN_POINT ( 'NONE',  ( 16.99647590252670426, 30.48934413892764894, -2.999999999999971578 ) ) ;
#21255 = VECTOR ( 'NONE', #16864, 1000.000000000000000 ) ;
#21256 = LINE ( 'NONE', #5334, #868 ) ;
#21257 = EDGE_CURVE ( 'NONE', #6602, #11475, #7961, .T. ) ;
#21258 = ORIENTED_EDGE ( 'NONE', *, *, #21359, .T. ) ;
#21259 = VERTEX_POINT ( 'NONE', #10856 ) ;
#21260 = VERTEX_POINT ( 'NONE', #11322 ) ;
#21261 = ORIENTED_EDGE ( 'NONE', *, *, #19323, .T. ) ;
#21262 = DIRECTION ( 'NONE',  ( -6.505213034913038160E-19, -3.903127820947822896E-18, -1.000000000000000000 ) ) ;
#21263 = DIRECTION ( 'NONE',  ( -0.000000000000000000, -1.000000000000000000, -0.000000000000000000 ) ) ;
#21264 = CARTESIAN_POINT ( 'NONE',  ( -14.85562396683486952, 32.28023859650867422, -3.000000000000005773 ) ) ;
#21265 = CYLINDRICAL_SURFACE ( 'NONE', #666, 3.399999999999995026 ) ;
#21266 = CARTESIAN_POINT ( 'NONE',  ( 2.098977200742791815, 39.97352556959325653, 50.29629763963205846 ) ) ;
#21267 = AXIS2_PLACEMENT_3D ( 'NONE', #5103, #13547, #17109 ) ;
#21268 = ORIENTED_EDGE ( 'NONE', *, *, #359, .T. ) ;
#21269 = CARTESIAN_POINT ( 'NONE',  ( 9.103081159019511759, 0.03030367950604059835, -53.87333532811884851 ) ) ;
#21270 = CARTESIAN_POINT ( 'NONE',  ( 31.67162468656012209, 14.67611967928900185, -2.999999999999971578 ) ) ;
#21271 = PRODUCT_DEFINITION_CONTEXT ( 'detailed design', #17787, 'design' ) ;
#21272 = DIRECTION ( 'NONE',  ( 0.000000000000000000, 0.000000000000000000, -1.000000000000000000 ) ) ;
#21273 = DIRECTION ( 'NONE',  ( 6.505213034913038160E-19, 3.903127820947822896E-18, 1.000000000000000000 ) ) ;
#21274 = CYLINDRICAL_SURFACE ( 'NONE', #11311, 9.000000000000003553 ) ;
#21275 = EDGE_CURVE ( 'NONE', #19009, #16507, #12681, .T. ) ;
#21276 = FACE_BOUND ( 'NONE', #3092, .T. ) ;
#21277 = AXIS2_PLACEMENT_3D ( 'NONE', #10414, #15233, #20528 ) ;
#21278 = AXIS2_PLACEMENT_3D ( 'NONE', #12149, #3458, #22370 ) ;
#21279 = FACE_OUTER_BOUND ( 'NONE', #695, .T. ) ;
#21280 = EDGE_CURVE ( 'NONE', #10118, #9571, #11976, .T. ) ;
#21281 = DIRECTION ( 'NONE',  ( 0.000000000000000000, 0.000000000000000000, -1.000000000000000000 ) ) ;
#21282 = ORIENTED_EDGE ( 'NONE', *, *, #19432, .T. ) ;
#21283 = ORIENTED_EDGE ( 'NONE', *, *, #501, .T. ) ;
#21284 = EDGE_CURVE ( 'NONE', #3548, #8759, #17829, .T. ) ;
#21285 = ORIENTED_EDGE ( 'NONE', *, *, #1103, .T. ) ;
#21286 = CARTESIAN_POINT ( 'NONE',  ( -0.1963897509086758586, -3.154216256251429318, -47.17168727994676658 ) ) ;
#21287 = DIRECTION ( 'NONE',  ( -0.000000000000000000, -0.000000000000000000, 1.000000000000000000 ) ) ;
#21288 = EDGE_CURVE ( 'NONE', #20345, #22114, #9150, .T. ) ;
#21289 = CIRCLE ( 'NONE', #5549, 59.99999999999703704 ) ;
#21290 = FACE_OUTER_BOUND ( 'NONE', #14689, .T. ) ;
#21291 = CARTESIAN_POINT ( 'NONE',  ( 23.65408649739145375, 22.22891329980533470, 3.000000000000016431 ) ) ;
#21292 = SHAPE_REPRESENTATION ( 'CASE', ( #18273 ), #10192 ) ;
#21293 = FACE_OUTER_BOUND ( 'NONE', #18839, .T. ) ;
#21294 = CARTESIAN_POINT ( 'NONE',  ( -14.58570206007863135, 6.310259562106216080, 59.03202081059066586 ) ) ;
#21295 = CARTESIAN_POINT ( 'NONE',  ( 31.92986134326236680, -18.22261011550291343, -2.800654218530485018 ) ) ;
#21296 = CYLINDRICAL_SURFACE ( 'NONE', #18488, 4.000000000000000000 ) ;
#21297 = ORIENTED_EDGE ( 'NONE', *, *, #22489, .T. ) ;
#21298 = DIRECTION ( 'NONE',  ( -6.505213034913038160E-19, -3.903127820947822896E-18, -1.000000000000000000 ) ) ;
#21299 = CARTESIAN_POINT ( 'NONE',  ( -7.928388824789384337, 38.36675580713608014, -56.15749817958554502 ) ) ;
#21300 = DIRECTION ( 'NONE',  ( -1.000000000000000000, -0.000000000000000000, -0.000000000000000000 ) ) ;
#21301 = DIRECTION ( 'NONE',  ( 0.000000000000000000, 0.000000000000000000, -1.000000000000000000 ) ) ;
#21302 = ORIENTED_EDGE ( 'NONE', *, *, #6032, .T. ) ;
#21303 = CARTESIAN_POINT ( 'NONE',  ( -35.00000000000000000, 0.000000000000000000, -49.99999999999997158 ) ) ;
#21304 = FACE_BOUND ( 'NONE', #15114, .T. ) ;
#21305 = DIRECTION ( 'NONE',  ( 0.000000000000000000, 1.000000000000000000, 0.000000000000000000 ) ) ;
#21306 =( REPRESENTATION_RELATIONSHIP ('NONE','NONE', #8442, #3430 ) REPRESENTATION_RELATIONSHIP_WITH_TRANSFORMATION ( #7331 )SHAPE_REPRESENTATION_RELATIONSHIP( ) );
#21307 = AXIS2_PLACEMENT_3D ( 'NONE', #14312, #17886, #14548 ) ;
#21308 = ORIENTED_EDGE ( 'NONE', *, *, #17441, .T. ) ;
#21309 = EDGE_CURVE ( 'NONE', #4860, #9803, #19675, .T. ) ;
#21310 = ORIENTED_EDGE ( 'NONE', *, *, #6010, .F. ) ;
#21311 = CARTESIAN_POINT ( 'NONE',  ( 2.220446049250313081E-13, -2.498001805406602216E-13, -6.859353255829918616 ) ) ;
#21312 = DIRECTION ( 'NONE',  ( 6.505213034913038160E-19, 3.903127820947822896E-18, 1.000000000000000000 ) ) ;
#21313 = ORIENTED_EDGE ( 'NONE', *, *, #21627, .F. ) ;
#21314 = CARTESIAN_POINT ( 'NONE',  ( 4.724946350300523916E-15, 8.251288694035745053, 0.000000000000000000 ) ) ;
#21315 = CARTESIAN_POINT ( 'NONE',  ( -12.27586057105639838, 4.193657236093905283, -55.54740530680978594 ) ) ;
#21316 = ORIENTED_EDGE ( 'NONE', *, *, #1810, .F. ) ;
#21317 = DIRECTION ( 'NONE',  ( 0.000000000000000000, 0.000000000000000000, -1.000000000000000000 ) ) ;
#21318 = DIRECTION ( 'NONE',  ( -1.000000000000000000, 0.000000000000000000, 0.000000000000000000 ) ) ;
#21319 = DIRECTION ( 'NONE',  ( 0.000000000000000000, 0.000000000000000000, -1.000000000000000000 ) ) ;
#21320 = AXIS2_PLACEMENT_3D ( 'NONE', #2753, #4705, #11219 ) ;
#21321 = FACE_OUTER_BOUND ( 'NONE', #8375, .T. ) ;
#21322 = ORIENTED_EDGE ( 'NONE', *, *, #17214, .F. ) ;
#21323 = CARTESIAN_POINT ( 'NONE',  ( 34.99999999999980815, 39.97500000000000142, 54.99999999999922551 ) ) ;
#21324 = CARTESIAN_POINT ( 'NONE',  ( -9.867969867547913054, 0.2954100743918419703, 54.30456930252528736 ) ) ;
#21325 = CARTESIAN_POINT ( 'NONE',  ( -9.689843208404459673, 39.33333333333334991, -54.54983754392748807 ) ) ;
#21326 = AXIS2_PLACEMENT_3D ( 'NONE', #11613, #6123, #15141 ) ;
#21327 = ORIENTED_EDGE ( 'NONE', *, *, #16160, .T. ) ;
#21328 = EDGE_CURVE ( 'NONE', #16891, #15727, #12693, .T. ) ;
#21329 = CARTESIAN_POINT ( 'NONE',  ( -17.99805307122284859, -21.44924440733170101, -4.999999999999984013 ) ) ;
#21330 = CARTESIAN_POINT ( 'NONE',  ( 9.689843208404422370, 39.33333333333334281, -54.54983754392748097 ) ) ;
#21331 = ADVANCED_FACE ( 'NONE', ( #5709 ), #10977, .T. ) ;
#21332 = ORIENTED_EDGE ( 'NONE', *, *, #14276, .F. ) ;
#21333 = AXIS2_PLACEMENT_3D ( 'NONE', #15297, #18646, #2951 ) ;
#21334 = EDGE_LOOP ( 'NONE', ( #4489, #8502, #9135, #21226 ) ) ;
#21335 = VERTEX_POINT ( 'NONE', #14465 ) ;
#21336 = AXIS2_PLACEMENT_3D ( 'NONE', #494, #21594, #7272 ) ;
#21337 = VECTOR ( 'NONE', #16884, 1000.000000000000000 ) ;
#21338 = EDGE_LOOP ( 'NONE', ( #9629, #9383, #1533, #6807 ) ) ;
#21339 = CARTESIAN_POINT ( 'NONE',  ( 35.00000000000001421, -5.000000000000000000, 1.540743955509788682E-30 ) ) ;
#21340 = CARTESIAN_POINT ( 'NONE',  ( 3.803764550617159124, 39.91204985064339184, -51.45951652639460150 ) ) ;
#21341 = CARTESIAN_POINT ( 'NONE',  ( 6.019227058680656661, 40.00000000000001421, 52.10376793666976170 ) ) ;
#21342 = ORIENTED_EDGE ( 'NONE', *, *, #9050, .F. ) ;
#21343 = CARTESIAN_POINT ( 'NONE',  ( -34.99999999999999289, -1.000000000000028644, -3.012171160963566127E-14 ) ) ;
#21344 = DIRECTION ( 'NONE',  ( 0.000000000000000000, -1.000000000000000000, 0.000000000000000000 ) ) ;
#21345 = EDGE_LOOP ( 'NONE', ( #11700, #10385, #11619, #21623, #1836, #2682, #5429 ) ) ;
#21346 = CARTESIAN_POINT ( 'NONE',  ( -2.587870662174074354, 0.1391398518287489672, 50.61865394279453767 ) ) ;
#21347 = CARTESIAN_POINT ( 'NONE',  ( 4.664299542270204193E-14, -2.819653587506501857, 47.26169151849854444 ) ) ;
#21348 = CARTESIAN_POINT ( 'NONE',  ( -14.93538271375398274, -34.13396246814581758, 3.000000000000023537 ) ) ;
#21349 = ORIENTED_EDGE ( 'NONE', *, *, #2200, .F. ) ;
#21350 = LINE ( 'NONE', #837, #18982 ) ;
#21351 = ORIENTED_EDGE ( 'NONE', *, *, #7358, .T. ) ;
#21352 = CARTESIAN_POINT ( 'NONE',  ( 3.171164708323686021, 39.94220383057359669, -51.05051439163197813 ) ) ;
#21353 = LINE ( 'NONE', #15738, #6817 ) ;
#21354 = B_SPLINE_CURVE_WITH_KNOTS ( 'NONE', 3,
 ( #14851, #18197, #5711, #7765 ),
 .UNSPECIFIED., .F., .F.,
 ( 4, 4 ),
 ( 9.545285769333515678E-07, 0.001900595205834842375 ),
 .UNSPECIFIED. ) ;
#21355 = LINE ( 'NONE', #19648, #18403 ) ;
#21356 = EDGE_LOOP ( 'NONE', ( #5951, #14397, #2219, #515 ) ) ;
#21357 = FACE_OUTER_BOUND ( 'NONE', #7616, .T. ) ;
#21358 = AXIS2_PLACEMENT_3D ( 'NONE', #16997, #1304, #15151 ) ;
#21359 = EDGE_CURVE ( 'NONE', #10824, #15170, #21501, .T. ) ;
#21360 = CARTESIAN_POINT ( 'NONE',  ( 19.96591191796975551, 18.54839033250521751, 58.13845218884756605 ) ) ;
#21361 = CARTESIAN_POINT ( 'NONE',  ( 26.64693883069180913, 24.43377932785589479, -2.933296326616372074 ) ) ;
#21362 = AXIS2_PLACEMENT_3D ( 'NONE', #12939, #14879, #6420 ) ;
#21363 = CIRCLE ( 'NONE', #10721, 50.00000000000001421 ) ;
#21364 = DIRECTION ( 'NONE',  ( -1.000000000000000000, 0.000000000000000000, 0.000000000000000000 ) ) ;
#21365 = EDGE_CURVE ( 'NONE', #15447, #2473, #19651, .T. ) ;
#21366 = ADVANCED_FACE ( 'NONE', ( #19107 ), #12516, .T. ) ;
#21368 = EDGE_CURVE ( 'NONE', #14834, #13710, #7209, .T. ) ;
#21367 = ORIENTED_EDGE ( 'NONE', *, *, #4464, .T. ) ;
#21369 = VECTOR ( 'NONE', #14148, 1000.000000000000000 ) ;
#21370 = ORIENTED_EDGE ( 'NONE', *, *, #2501, .F. ) ;
#21371 = VERTEX_POINT ( 'NONE', #15532 ) ;
#21372 = ORIENTED_EDGE ( 'NONE', *, *, #7133, .T. ) ;
#21373 = PLANE ( 'NONE',  #19120 ) ;
#21374 = CARTESIAN_POINT ( 'NONE',  ( -3.418729828831206752E-14, 1.500000000000004885, 15.99999999999970512 ) ) ;
#21375 = AXIS2_PLACEMENT_3D ( 'NONE', #1019, #3201, #11561 ) ;
#21376 = CARTESIAN_POINT ( 'NONE',  ( 0.000000000000000000, 30.00000000000000355, 4.025000000000000355 ) ) ;
#21377 = ADVANCED_FACE ( 'NONE', ( #21357 ), #5030, .F. ) ;
#21378 = VERTEX_POINT ( 'NONE', #3954 ) ;
#21379 = CARTESIAN_POINT ( 'NONE',  ( 31.41173278719261575, 17.66631876130911394, -6.999999999999950262 ) ) ;
#21380 = DIRECTION ( 'NONE',  ( 0.000000000000000000, 0.000000000000000000, -1.000000000000000000 ) ) ;
#21381 = AXIS2_PLACEMENT_3D ( 'NONE', #5620, #3919, #10889 ) ;
#21382 = ORIENTED_EDGE ( 'NONE', *, *, #12806, .T. ) ;
#21383 = CARTESIAN_POINT ( 'NONE',  ( -35.00000000000000000, -9.000000000000001776, -13.99999999999998579 ) ) ;
#21384 = CARTESIAN_POINT ( 'NONE',  ( 13.85640646055130709, 1.500000000000004885, -8.000000000000097700 ) ) ;
#21385 = CARTESIAN_POINT ( 'NONE',  ( 2.602085213965210642E-15, 5.025303850726727362, 19.00000000000000355 ) ) ;
#21386 = CARTESIAN_POINT ( 'NONE',  ( 13.00000000000024336, -2.516660498395250745, 105.0000000000000142 ) ) ;
#21387 = AXIS2_PLACEMENT_3D ( 'NONE', #8508, #337, #15485 ) ;
#21388 = DIRECTION ( 'NONE',  ( -0.000000000000000000, -1.000000000000000000, -0.000000000000000000 ) ) ;
#21389 = CARTESIAN_POINT ( 'NONE',  ( -35.00000000000000000, 40.00000000000000000, 1.387778780781445676E-14 ) ) ;
#21390 = CARTESIAN_POINT ( 'NONE',  ( -1.387778780781445518E-14, 20.00000000000000355, -105.0000000000000142 ) ) ;
#21391 = VECTOR ( 'NONE', #3361, 1000.000000000000000 ) ;
#21392 = VERTEX_POINT ( 'NONE', #20834 ) ;
#21393 = ORIENTED_EDGE ( 'NONE', *, *, #6289, .F. ) ;
#21394 = ADVANCED_FACE ( 'NONE', ( #22556 ), #20710, .F. ) ;
#21395 = ORIENTED_EDGE ( 'NONE', *, *, #1493, .F. ) ;
#21396 = DIRECTION ( 'NONE',  ( -1.000000000000000000, -1.208970125616063644E-17, 0.000000000000000000 ) ) ;
#21397 = EDGE_CURVE ( 'NONE', #16345, #7411, #14290, .T. ) ;
#21398 = VECTOR ( 'NONE', #181, 1000.000000000000114 ) ;
#21399 = CARTESIAN_POINT ( 'NONE',  ( 2.775557561562891351E-14, -2.775557561562891351E-14, 2.999999999999999112 ) ) ;
#21400 = CARTESIAN_POINT ( 'NONE',  ( 22.12933039895921894, -2.999999999999998668, 2.710061364035962525E-15 ) ) ;
#21401 = CARTESIAN_POINT ( 'NONE',  ( -34.99999999999980815, 26.00000000000000355, 54.99999999999922551 ) ) ;
#21402 = EDGE_CURVE ( 'NONE', #2004, #19351, #14000, .T. ) ;
#21403 = DIRECTION ( 'NONE',  ( -0.000000000000000000, 1.000000000000000000, -0.000000000000000000 ) ) ;
#21404 = DIRECTION ( 'NONE',  ( -0.000000000000000000, 1.000000000000000000, -0.000000000000000000 ) ) ;
#21405 = CARTESIAN_POINT ( 'NONE',  ( -17.76477806472196974, 33.73774409953113462, -57.47211831788180803 ) ) ;
#21406 = DIRECTION ( 'NONE',  ( 0.000000000000000000, 0.000000000000000000, 1.000000000000000000 ) ) ;
#21407 = ORIENTED_EDGE ( 'NONE', *, *, #13116, .F. ) ;
#21408 = CARTESIAN_POINT ( 'NONE',  ( 13.85640646055130709, -1.500000000000015099, -8.000000000000097700 ) ) ;
#21409 = DIRECTION ( 'NONE',  ( -0.000000000000000000, -1.000000000000000000, -0.000000000000000000 ) ) ;
#21410 = DIRECTION ( 'NONE',  ( -1.000000000000000000, -1.208970125616081209E-17, 0.000000000000000000 ) ) ;
#21411 = CARTESIAN_POINT ( 'NONE',  ( -22.97438720605751783, 22.98755168577401520, 3.000000000000023537 ) ) ;
#21412 = ORIENTED_EDGE ( 'NONE', *, *, #9545, .T. ) ;
#21413 = AXIS2_PLACEMENT_3D ( 'NONE', #3331, #17394, #17277 ) ;
#21414 = LINE ( 'NONE', #14407, #5665 ) ;
#21415 = LINE ( 'NONE', #2171, #8291 ) ;
#21416 = CARTESIAN_POINT ( 'NONE',  ( 14.89439646620657953, 6.624450698088172551, -59.14252023619225440 ) ) ;
#21417 = CIRCLE ( 'NONE', #5313, 60.00000000000000000 ) ;
#21418 = EDGE_LOOP ( 'NONE', ( #12948, #247, #21679, #3422, #8748, #13648 ) ) ;
#21419 = CYLINDRICAL_SURFACE ( 'NONE', #3452, 49.99999999999998579 ) ;
#21420 = SHAPE_REPRESENTATION ( 'FLYWHEEL', ( #18273 ), #1444 ) ;
#21421 = AXIS2_PLACEMENT_3D ( 'NONE', #5089, #8175, #10219 ) ;
#21422 = ORIENTED_EDGE ( 'NONE', *, *, #9598, .T. ) ;
#21423 = CARTESIAN_POINT ( 'NONE',  ( -1.568459684869329074, 24.67391323485165699, 6.880481854261958574 ) ) ;
#21424 = AXIS2_PLACEMENT_3D ( 'NONE', #10127, #20354, #22185 ) ;
#21425 = FACE_BOUND ( 'NONE', #4490, .T. ) ;
#21426 = CARTESIAN_POINT ( 'NONE',  ( 2.775557561562891351E-14, 2.775557561562891351E-14, 5.750000000000001776 ) ) ;
#21427 = EDGE_LOOP ( 'NONE', ( #6347, #5708, #4483, #4399 ) ) ;
#21428 = FACE_BOUND ( 'NONE', #19106, .T. ) ;
#21429 = CARTESIAN_POINT ( 'NONE',  ( -9.744263423232260024, 2.495070046662454466, -54.63687069582701383 ) ) ;
#21430 = ORIENTED_EDGE ( 'NONE', *, *, #16805, .T. ) ;
#21431 = DIRECTION ( 'NONE',  ( 0.000000000000000000, 0.000000000000000000, 1.000000000000000000 ) ) ;
#21432 = AXIS2_PLACEMENT_3D ( 'NONE', #8729, #19050, #12163 ) ;
#21433 = DIRECTION ( 'NONE',  ( 0.000000000000000000, 0.000000000000000000, -1.000000000000000000 ) ) ;
#21434 = CARTESIAN_POINT ( 'NONE',  ( -9.952189117650897643, 40.00000000000000000, 53.64426396172076039 ) ) ;
#21435 = CIRCLE ( 'NONE', #1684, 4.000000000000000000 ) ;
#21436 = DIRECTION ( 'NONE',  ( 0.000000000000000000, -1.000000000000000000, 0.000000000000000000 ) ) ;
#21437 = ORIENTED_EDGE ( 'NONE', *, *, #15894, .F. ) ;
#21438 = FACE_OUTER_BOUND ( 'NONE', #3961, .T. ) ;
#21439 = CARTESIAN_POINT ( 'NONE',  ( -7.505578006075202424, 1.461761173328241181, 55.63523492904089096 ) ) ;
#21440 = CARTESIAN_POINT ( 'NONE',  ( -0.5103191905027275599, 39.99845979207320568, -49.12706114568621985 ) ) ;
#21441 = EDGE_CURVE ( 'NONE', #15404, #13475, #8314, .T. ) ;
#21442 = ORIENTED_EDGE ( 'NONE', *, *, #21744, .T. ) ;
#21443 = CARTESIAN_POINT ( 'NONE',  ( 24.65063509461090518, 12.50000000000006750, 2.999999999999995559 ) ) ;
#21444 = CARTESIAN_POINT ( 'NONE',  ( 34.99999999999980815, 40.00000000000000000, 52.49999999999922551 ) ) ;
#21445 = AXIS2_PLACEMENT_3D ( 'NONE', #883, #17026, #15301 ) ;
#21446 = VECTOR ( 'NONE', #14608, 1000.000000000000000 ) ;
#21447 = CIRCLE ( 'NONE', #20002, 58.99999999999699440 ) ;
#21448 = ADVANCED_FACE ( 'NONE', ( #19824 ), #11213, .F. ) ;
#21449 = ORIENTED_EDGE ( 'NONE', *, *, #22654, .T. ) ;
#21450 = AXIS2_PLACEMENT_3D ( 'NONE', #12116, #20597, #5027 ) ;
#21451 = EDGE_LOOP ( 'NONE', ( #1360, #19775 ) ) ;
#21452 = ORIENTED_EDGE ( 'NONE', *, *, #19281, .F. ) ;
#21453 = ORIENTED_EDGE ( 'NONE', *, *, #3623, .T. ) ;
#21454 = CARTESIAN_POINT ( 'NONE',  ( -25.34312177887347417, 20.17230487860832611, 3.000000000000006217 ) ) ;
#21455 = DIRECTION ( 'NONE',  ( -1.000000000000000000, 1.275531967630005245E-16, 0.000000000000000000 ) ) ;
#21456 = CARTESIAN_POINT ( 'NONE',  ( -90.00000000000000000, 26.00000000000000355, -9.108981535246192915E-16 ) ) ;
#21457 = CARTESIAN_POINT ( 'NONE',  ( 2.999999999999997780, 15.99999999999999645, 8.485281374238567764 ) ) ;
#21458 = ADVANCED_FACE ( 'NONE', ( #11446 ), #18433, .F. ) ;
#21459 = ORIENTED_EDGE ( 'NONE', *, *, #5227, .F. ) ;
#21460 = FACE_OUTER_BOUND ( 'NONE', #7129, .T. ) ;
#21461 = CARTESIAN_POINT ( 'NONE',  ( 20.00000000000004974, -2.506448799221099482E-14, 2.999999999999995559 ) ) ;
#21462 = EDGE_LOOP ( 'NONE', ( #2085, #15775, #15489, #17364 ) ) ;
#21463 = CARTESIAN_POINT ( 'NONE',  ( -2.949288349266179665, -1.205118272524452916, 50.23218672884134861 ) ) ;
#21464 = CIRCLE ( 'NONE', #17052, 20.00000000000000000 ) ;
#21465 = CARTESIAN_POINT ( 'NONE',  ( 12.00000000000000355, 12.49999999999999467, 1.469576158976823947E-15 ) ) ;
#21466 = CARTESIAN_POINT ( 'NONE',  ( 13.83143812983136911, -29.36548507648045714, -2.999999999999971578 ) ) ;
#21467 = EDGE_LOOP ( 'NONE', ( #9902, #6855, #12421, #12760 ) ) ;
#21468 = CARTESIAN_POINT ( 'NONE',  ( 1.145276119296964268, 0.005126887279929492891, 49.65522505680549870 ) ) ;
#21469 = ORIENTED_EDGE ( 'NONE', *, *, #21827, .T. ) ;
#21470 = CARTESIAN_POINT ( 'NONE',  ( 4.628075497661852999, 39.46063506869896997, 53.65703709785807263 ) ) ;
#21471 = ADVANCED_FACE ( 'NONE', ( #21653 ), #4125, .F. ) ;
#21472 = CYLINDRICAL_SURFACE ( 'NONE', #3904, 15.00000000000000000 ) ;
#21473 = DIRECTION ( 'NONE',  ( 6.505213034913038160E-19, 3.903127820947822896E-18, 1.000000000000000000 ) ) ;
#21474 = DIRECTION ( 'NONE',  ( -0.000000000000000000, -0.000000000000000000, -1.000000000000000000 ) ) ;
#21475 = CIRCLE ( 'NONE', #3174, 12.00000000000000000 ) ;
#21476 = ORIENTED_EDGE ( 'NONE', *, *, #5407, .F. ) ;
#21477 = CARTESIAN_POINT ( 'NONE',  ( 18.87679372942819001, 13.33229001579472417, 60.34430474298743263 ) ) ;
#21478 = DIRECTION ( 'NONE',  ( -0.000000000000000000, -0.000000000000000000, -1.000000000000000000 ) ) ;
#21479 = ADVANCED_FACE ( 'NONE', ( #16256 ), #13048, .F. ) ;
#21480 = DIRECTION ( 'NONE',  ( 0.000000000000000000, 1.000000000000000000, 0.000000000000000000 ) ) ;
#21481 = AXIS2_PLACEMENT_3D ( 'NONE', #11576, #18788, #18564 ) ;
#21482 = ORIENTED_EDGE ( 'NONE', *, *, #6945, .F. ) ;
#21483 = VERTEX_POINT ( 'NONE', #9397 ) ;
#21484 = ORIENTED_EDGE ( 'NONE', *, *, #18522, .F. ) ;
#21485 = EDGE_LOOP ( 'NONE', ( #22352, #2068, #21831, #20661 ) ) ;
#21486 = DIRECTION ( 'NONE',  ( 0.000000000000000000, 0.000000000000000000, -1.000000000000000000 ) ) ;
#21487 = DIRECTION ( 'NONE',  ( -1.445602896647339163E-16, 0.000000000000000000, -1.000000000000000000 ) ) ;
#21488 = CARTESIAN_POINT ( 'NONE',  ( 23.74488952252792728, -25.58633464742643326, 2.999999999999999112 ) ) ;
#21489 = EDGE_CURVE ( 'NONE', #19293, #12403, #2834, .T. ) ;
#21490 = ORIENTED_EDGE ( 'NONE', *, *, #8090, .T. ) ;
#21491 = CARTESIAN_POINT ( 'NONE',  ( 13.85640646055130709, -25.00000000000000000, -8.000000000000097700 ) ) ;
#21492 = DIRECTION ( 'NONE',  ( -1.000000000000000000, 1.301042606982605814E-16, 0.000000000000000000 ) ) ;
#21493 = AXIS2_PLACEMENT_3D ( 'NONE', #13893, #20908, #4281 ) ;
#21494 = ORIENTED_EDGE ( 'NONE', *, *, #7208, .F. ) ;
#21495 = FACE_BOUND ( 'NONE', #10548, .T. ) ;
#21496 = VECTOR ( 'NONE', #4062, 1000.000000000000000 ) ;
#21497 = CARTESIAN_POINT ( 'NONE',  ( 29.99999999999998579, 20.00000000000000711, 105.0000000000000142 ) ) ;
#21498 = EDGE_CURVE ( 'NONE', #2350, #4971, #15627, .T. ) ;
#21499 = CARTESIAN_POINT ( 'NONE',  ( 36.06598984771572702, 10.00000000000000000, -48.42385786802028491 ) ) ;
#21500 = EDGE_CURVE ( 'NONE', #11128, #16827, #16490, .T. ) ;
#21501 = CIRCLE ( 'NONE', #10131, 36.76383501243555685 ) ;
#21502 = DIRECTION ( 'NONE',  ( 0.000000000000000000, 0.000000000000000000, 1.000000000000000000 ) ) ;
#21503 = CARTESIAN_POINT ( 'NONE',  ( -28.06260833510301822, 14.30873905802315704, -6.999999999999950262 ) ) ;
#21504 = CARTESIAN_POINT ( 'NONE',  ( -1.706267410340174185E-14, 40.00000000000000000, 48.73397172404484223 ) ) ;
#21505 = VECTOR ( 'NONE', #10321, 1000.000000000000000 ) ;
#21506 = CIRCLE ( 'NONE', #12699, 1.000000000000000888 ) ;
#21507 = DIRECTION ( 'NONE',  ( 6.505213034913038160E-19, 3.903127820947822896E-18, 1.000000000000000000 ) ) ;
#21508 = EDGE_CURVE ( 'NONE', #16292, #12719, #5756, .T. ) ;
#21509 = ORIENTED_EDGE ( 'NONE', *, *, #13711, .F. ) ;
#21510 = AXIS2_PLACEMENT_3D ( 'NONE', #20506, #13038, #18220 ) ;
#21511 = ORIENTED_EDGE ( 'NONE', *, *, #9181, .T. ) ;
#21512 = AXIS2_PLACEMENT_3D ( 'NONE', #3065, #10036, #15649 ) ;
#21513 = AXIS2_PLACEMENT_3D ( 'NONE', #9371, #20141, #12895 ) ;
#21514 = ORIENTED_EDGE ( 'NONE', *, *, #3105, .F. ) ;
#21515 = CARTESIAN_POINT ( 'NONE',  ( -35.00000000000058265, 28.00000000000000000, -55.00000000000076028 ) ) ;
#21516 = EDGE_CURVE ( 'NONE', #1894, #12579, #15988, .T. ) ;
#21517 = DIRECTION ( 'NONE',  ( 0.000000000000000000, 0.000000000000000000, 1.000000000000000000 ) ) ;
#21518 = CARTESIAN_POINT ( 'NONE',  ( 42.50000000000000711, -12.00000000000012434, 47.50000000000000711 ) ) ;
#21519 = CARTESIAN_POINT ( 'NONE',  ( 0.7857880201000516651, 12.99916404495074040, 7.000278651543345276 ) ) ;
#21520 = AXIS2_PLACEMENT_3D ( 'NONE', #12389, #125, #12600 ) ;
#21521 = DIRECTION ( 'NONE',  ( -0.000000000000000000, -1.000000000000000000, -0.000000000000000000 ) ) ;
#21522 = DIRECTION ( 'NONE',  ( -0.000000000000000000, -1.000000000000000000, -0.000000000000000000 ) ) ;
#21523 = CARTESIAN_POINT ( 'NONE',  ( -13.88612301964757201, 34.41939562427583610, -58.78253654025285613 ) ) ;
#21524 = FACE_OUTER_BOUND ( 'NONE', #2549, .T. ) ;
#21525 = AXIS2_PLACEMENT_3D ( 'NONE', #10910, #2213, #9316 ) ;
#21526 = ORIENTED_EDGE ( 'NONE', *, *, #13368, .T. ) ;
#21527 = AXIS2_PLACEMENT_3D ( 'NONE', #21384, #6963, #12217 ) ;
#21528 = CARTESIAN_POINT ( 'NONE',  ( -22.15900668633764781, -29.33526866242125308, -1.999999999999980904 ) ) ;
#21529 = CARTESIAN_POINT ( 'NONE',  ( -12.99999999999980282, -2.516660498395516310, 60.00099999999999767 ) ) ;
#21530 = CARTESIAN_POINT ( 'NONE',  ( 34.99999999999980815, 40.00000000000000711, 52.47499999999922693 ) ) ;
#21531 = CARTESIAN_POINT ( 'NONE',  ( 8.199064559763693083, 7.360541284256873595, -42.22991907770646947 ) ) ;
#21532 = CONICAL_SURFACE ( 'NONE', #11271, 4.025000000000000355, 0.7853981633974136400 ) ;
#21533 = EDGE_CURVE ( 'NONE', #66, #19404, #20408, .T. ) ;
#21534 = VERTEX_POINT ( 'NONE', #8573 ) ;
#21535 = DIRECTION ( 'NONE',  ( 6.505213034913038160E-19, 3.903127820947822896E-18, 1.000000000000000000 ) ) ;
#21536 = DIRECTION ( 'NONE',  ( 1.000000000000000000, 2.269002777743560714E-17, 0.000000000000000000 ) ) ;
#21537 = DIRECTION ( 'NONE',  ( -0.000000000000000000, -0.000000000000000000, 1.000000000000000000 ) ) ;
#21538 = CIRCLE ( 'NONE', #1420, 1.000000000000000888 ) ;
#21539 = EDGE_CURVE ( 'NONE', #11046, #9968, #1742, .T. ) ;
#21540 = B_SPLINE_CURVE_WITH_KNOTS ( 'NONE', 3,
 ( #7222, #5733, #14542, #14191 ),
 .UNSPECIFIED., .F., .F.,
 ( 4, 4 ),
 ( 9.715086407228946956E-07, 0.001929643240672380446 ),
 .UNSPECIFIED. ) ;
#21541 = AXIS2_PLACEMENT_3D ( 'NONE', #12475, #17643, #5609 ) ;
#21542 = EDGE_LOOP ( 'NONE', ( #15617, #16661, #451, #14651 ) ) ;
#21543 = AXIS2_PLACEMENT_3D ( 'NONE', #3403, #1680, #5344 ) ;
#21544 = DIRECTION ( 'NONE',  ( 0.000000000000000000, 0.000000000000000000, 1.000000000000000000 ) ) ;
#21545 = CARTESIAN_POINT ( 'NONE',  ( 7.349642776635462837, 39.99999999999999289, -52.69668487371527732 ) ) ;
#21546 = VECTOR ( 'NONE', #12473, 1000.000000000000000 ) ;
#21547 = ORIENTED_EDGE ( 'NONE', *, *, #12380, .F. ) ;
#21548 = CARTESIAN_POINT ( 'NONE',  ( 4.274780932708218018, 39.88689858671455113, -51.75995564879541888 ) ) ;
#21549 = CYLINDRICAL_SURFACE ( 'NONE', #6965, 3.999999999999997335 ) ;
#21550 = LINE ( 'NONE', #7104, #21546 ) ;
#21551 = ORIENTED_EDGE ( 'NONE', *, *, #19229, .T. ) ;
#21552 = CARTESIAN_POINT ( 'NONE',  ( 2.602085213965210642E-15, 0.000000000000000000, 0.000000000000000000 ) ) ;
#21553 = CARTESIAN_POINT ( 'NONE',  ( -6.122940801430958757, 40.00000000000000000, 52.15215292453424922 ) ) ;
#21554 = EDGE_LOOP ( 'NONE', ( #14773, #9417 ) ) ;
#21555 = DIRECTION ( 'NONE',  ( -0.000000000000000000, -1.000000000000000000, -0.000000000000000000 ) ) ;
#21556 = CARTESIAN_POINT ( 'NONE',  ( 42.50000000000000711, -5.000000000000000000, 47.50000000000000711 ) ) ;
#21557 = FACE_OUTER_BOUND ( 'NONE', #10866, .T. ) ;
#21558 = DIRECTION ( 'NONE',  ( 6.505213034913038160E-19, 3.903127820947822896E-18, 1.000000000000000000 ) ) ;
#21559 = VERTEX_POINT ( 'NONE', #22571 ) ;
#21560 = DIRECTION ( 'NONE',  ( 0.000000000000000000, -1.000000000000000000, 0.000000000000000000 ) ) ;
#21561 = FACE_BOUND ( 'NONE', #12481, .T. ) ;
#21562 = CIRCLE ( 'NONE', #9488, 2.499999999999995115 ) ;
#21563 = CARTESIAN_POINT ( 'NONE',  ( -9.075375600668062148, 39.43595020880619728, -54.33405310382095621 ) ) ;
#21564 = EDGE_CURVE ( 'NONE', #13818, #18812, #6495, .T. ) ;
#21565 = VERTEX_POINT ( 'NONE', #5154 ) ;
#21566 = CARTESIAN_POINT ( 'NONE',  ( -8.199064559763614923, 32.63945871574321700, 42.22991907770644104 ) ) ;
#21567 = DIRECTION ( 'NONE',  ( -6.505213034913038160E-19, -3.903127820947822896E-18, -1.000000000000000000 ) ) ;
#21568 = PRODUCT_DEFINITION_FORMATION_WITH_SPECIFIED_SOURCE ( 'ANY', '', #891, .NOT_KNOWN. ) ;
#21569 = ADVANCED_FACE ( 'NONE', ( #18892 ), #10167, .T. ) ;
#21570 = ORIENTED_EDGE ( 'NONE', *, *, #10006, .F. ) ;
#21571 = ORIENTED_EDGE ( 'NONE', *, *, #2720, .T. ) ;
#21572 = AXIS2_PLACEMENT_3D ( 'NONE', #17122, #8532, #22529 ) ;
#21573 = EDGE_LOOP ( 'NONE', ( #12553, #3261, #3856, #10409 ) ) ;
#21574 = EDGE_CURVE ( 'NONE', #43, #11353, #10500, .T. ) ;
#21575 = ORIENTED_EDGE ( 'NONE', *, *, #17655, .T. ) ;
#21576 = CARTESIAN_POINT ( 'NONE',  ( 6.000000000000000000, 20.00000000000000000, 5.999999999999999112 ) ) ;
#21577 = DIRECTION ( 'NONE',  ( -6.505213034913038160E-19, -3.903127820947822896E-18, -1.000000000000000000 ) ) ;
#21578 = CARTESIAN_POINT ( 'NONE',  ( -4.163336342344415913E-14, 40.00000000000002132, -48.73397172404479250 ) ) ;
#21579 = DIRECTION ( 'NONE',  ( 6.505213034913038160E-19, 3.903127820947822896E-18, 1.000000000000000000 ) ) ;
#21580 = LINE ( 'NONE', #2445, #17501 ) ;
#21581 = ORIENTED_EDGE ( 'NONE', *, *, #21711, .F. ) ;
#21582 = DIRECTION ( 'NONE',  ( -9.251858538543433311E-16, 0.000000000000000000, 1.000000000000000000 ) ) ;
#21583 = DIRECTION ( 'NONE',  ( -1.000000000000000000, 0.000000000000000000, 0.000000000000000000 ) ) ;
#21584 = VERTEX_POINT ( 'NONE', #13371 ) ;
#21585 = DIRECTION ( 'NONE',  ( -0.000000000000000000, -1.000000000000000000, -0.000000000000000000 ) ) ;
#21586 = DIRECTION ( 'NONE',  ( -1.000000000000000000, 0.000000000000000000, -0.000000000000000000 ) ) ;
#21587 = EDGE_CURVE ( 'NONE', #8689, #3941, #8328, .T. ) ;
#21588 = LINE ( 'NONE', #1990, #20381 ) ;
#21589 = ORIENTED_EDGE ( 'NONE', *, *, #17169, .T. ) ;
#21590 = CARTESIAN_POINT ( 'NONE',  ( 1.591932335265033587E-15, -4.923002280079127832E-27, 50.50395615645412306 ) ) ;
#21591 = ORIENTED_EDGE ( 'NONE', *, *, #11384, .T. ) ;
#21592 = FACE_OUTER_BOUND ( 'NONE', #967, .T. ) ;
#21593 = FILL_AREA_STYLE ('',( #8032 ) ) ;
#21594 = DIRECTION ( 'NONE',  ( 1.296372316667914327E-16, 1.000000000000000000, -0.000000000000000000 ) ) ;
#21595 = ORIENTED_EDGE ( 'NONE', *, *, #6597, .T. ) ;
#21596 = AXIS2_PLACEMENT_3D ( 'NONE', #10567, #17566, #9313 ) ;
#21597 = CARTESIAN_POINT ( 'NONE',  ( 15.13173276104727094, 33.09480349269512089, 56.64473394289761643 ) ) ;
#21598 = CARTESIAN_POINT ( 'NONE',  ( 35.00000000000000000, -4.928932188134504955, 4.258610482196280173E-15 ) ) ;
#21599 = CYLINDRICAL_SURFACE ( 'NONE', #1240, 2.099999999999997868 ) ;
#21600 = VERTEX_POINT ( 'NONE', #6629 ) ;
#21601 = AXIS2_PLACEMENT_3D ( 'NONE', #20872, #1504, #17414 ) ;
#21602 = ORIENTED_EDGE ( 'NONE', *, *, #2596, .T. ) ;
#21603 = ORIENTED_EDGE ( 'NONE', *, *, #8868, .F. ) ;
#21604 = VERTEX_POINT ( 'NONE', #10280 ) ;
#21605 = CYLINDRICAL_SURFACE ( 'NONE', #11442, 1.000000000000000888 ) ;
#21606 = DIRECTION ( 'NONE',  ( -0.000000000000000000, 1.000000000000000000, -0.000000000000000000 ) ) ;
#21607 = DIRECTION ( 'NONE',  ( 0.000000000000000000, 1.000000000000000000, -0.000000000000000000 ) ) ;
#21608 = CONICAL_SURFACE ( 'NONE', #11722, 34.00000000000000000, 1.308996938995746095 ) ;
#21609 = ORIENTED_EDGE ( 'NONE', *, *, #19179, .T. ) ;
#21610 = CARTESIAN_POINT ( 'NONE',  ( -35.99819890246949683, 7.463862311151203244, -2.800654218530485018 ) ) ;
#21611 = CARTESIAN_POINT ( 'NONE',  ( 35.00000000000000000, -4.999999999999997335, 4.258610482196280173E-15 ) ) ;
#21612 = EDGE_CURVE ( 'NONE', #15098, #13932, #11633, .T. ) ;
#21613 = ORIENTED_EDGE ( 'NONE', *, *, #16396, .F. ) ;
#21614 = CARTESIAN_POINT ( 'NONE',  ( -42.49999999999996447, 10.00000000000000000, -50.00000000000000711 ) ) ;
#21615 = DIRECTION ( 'NONE',  ( -6.505213034913038160E-19, -3.903127820947822896E-18, -1.000000000000000000 ) ) ;
#21616 = DIRECTION ( 'NONE',  ( -6.505213034913038160E-19, -3.903127820947822896E-18, -1.000000000000000000 ) ) ;
#21617 = DIRECTION ( 'NONE',  ( 1.000000000000000000, 0.000000000000000000, -1.224646799147353207E-16 ) ) ;
#21618 = AXIS2_PLACEMENT_3D ( 'NONE', #2157, #424, #6981 ) ;
#21619 = CARTESIAN_POINT ( 'NONE',  ( 3.460816278822046447E-15, -1.500000000000011768, 0.000000000000000000 ) ) ;
#21620 = CARTESIAN_POINT ( 'NONE',  ( 35.00000000000000000, 0.000000000000000000, 52.49999999999698019 ) ) ;
#21621 = ADVANCED_FACE ( 'NONE', ( #1359 ), #15430, .T. ) ;
#21622 = DIRECTION ( 'NONE',  ( 6.505213034913038160E-19, 3.903127820947822896E-18, 1.000000000000000000 ) ) ;
#21623 = ORIENTED_EDGE ( 'NONE', *, *, #20572, .F. ) ;
#21624 = VERTEX_POINT ( 'NONE', #15204 ) ;
#21625 = VECTOR ( 'NONE', #4535, 1000.000000000000000 ) ;
#21626 = EDGE_CURVE ( 'NONE', #12299, #14267, #18584, .T. ) ;
#21627 = EDGE_CURVE ( 'NONE', #14890, #4617, #13807, .T. ) ;
#21628 = ORIENTED_EDGE ( 'NONE', *, *, #7352, .F. ) ;
#21629 = CARTESIAN_POINT ( 'NONE',  ( 3.469446951953614189E-15, -0.9047447100419790944, 18.42595423422130452 ) ) ;
#21630 = AXIS2_PLACEMENT_3D ( 'NONE', #18958, #6586, #3147 ) ;
#21631 = CARTESIAN_POINT ( 'NONE',  ( 15.49999999999993960, 42.51666049839543149, -100.0000000000000000 ) ) ;
#21632 = DIRECTION ( 'NONE',  ( 0.000000000000000000, 1.000000000000000000, 0.000000000000000000 ) ) ;
#21633 = CARTESIAN_POINT ( 'NONE',  ( -12.09218358684866423, 1.291952833854532079, -55.42846997241218077 ) ) ;
#21634 = CARTESIAN_POINT ( 'NONE',  ( -7.704815895020981742, 39.66337687413038537, -53.66058441934326595 ) ) ;
#21635 = DIRECTION ( 'NONE',  ( -0.000000000000000000, -0.000000000000000000, -1.000000000000000000 ) ) ;
#21636 = CIRCLE ( 'NONE', #21278, 19.11328065563151668 ) ;
#21637 = ORIENTED_EDGE ( 'NONE', *, *, #9134, .T. ) ;
#21638 = DIRECTION ( 'NONE',  ( 0.000000000000000000, 0.000000000000000000, 1.000000000000000000 ) ) ;
#21639 = CARTESIAN_POINT ( 'NONE',  ( -4.589682443554583102, 39.46972628399738880, -53.62209933471819312 ) ) ;
#21640 = CARTESIAN_POINT ( 'NONE',  ( 3.330669073875469621E-13, -1.110223024625156540E-13, -2.999999999999971578 ) ) ;
#21641 = CARTESIAN_POINT ( 'NONE',  ( 2.220446049250313081E-13, 2.775557561562891351E-14, -2.800654218530485018 ) ) ;
#21642 = ORIENTED_EDGE ( 'NONE', *, *, #9506, .F. ) ;
#21643 = DIRECTION ( 'NONE',  ( -0.000000000000000000, -0.000000000000000000, 1.000000000000000000 ) ) ;
#21644 = VERTEX_POINT ( 'NONE', #20726 ) ;
#21645 = EDGE_CURVE ( 'NONE', #12891, #11565, #5034, .T. ) ;
#21646 = CARTESIAN_POINT ( 'NONE',  ( -6.696867368503558448E-15, 40.00000000000000000, -48.73397172404479960 ) ) ;
#21647 = DIRECTION ( 'NONE',  ( -1.000000000000000000, 0.000000000000000000, 0.000000000000000000 ) ) ;
#21648 = EDGE_CURVE ( 'NONE', #19879, #18120, #17483, .T. ) ;
#21649 = EDGE_CURVE ( 'NONE', #16333, #11887, #15262, .T. ) ;
#21650 = ORIENTED_EDGE ( 'NONE', *, *, #18911, .T. ) ;
#21651 = DIRECTION ( 'NONE',  ( -1.000000000000000000, 0.000000000000000000, 0.000000000000000000 ) ) ;
#21652 = AXIS2_PLACEMENT_3D ( 'NONE', #7474, #9084, #19749 ) ;
#21653 = FACE_OUTER_BOUND ( 'NONE', #19300, .T. ) ;
#21654 = EDGE_LOOP ( 'NONE', ( #6001, #5199 ) ) ;
#21655 = CARTESIAN_POINT ( 'NONE',  ( 0.5260908555861737446, 39.99836280959126356, -49.13907560113233330 ) ) ;
#21656 = DIRECTION ( 'NONE',  ( 0.000000000000000000, 1.000000000000000000, 0.000000000000000000 ) ) ;
#21657 = DIRECTION ( 'NONE',  ( -1.000000000000000000, 1.530638361156006492E-16, 0.000000000000000000 ) ) ;
#21658 = ADVANCED_FACE ( 'NONE', ( #18671 ), #2976, .F. ) ;
#21659 = ORIENTED_EDGE ( 'NONE', *, *, #3436, .F. ) ;
#21660 = CYLINDRICAL_SURFACE ( 'NONE', #16563, 31.50000000000000711 ) ;
#21661 = DIRECTION ( 'NONE',  ( 6.505213034913038160E-19, 3.903127820947822896E-18, 1.000000000000000000 ) ) ;
#21662 = ORIENTED_EDGE ( 'NONE', *, *, #12062, .F. ) ;
#21663 = CARTESIAN_POINT ( 'NONE',  ( -42.50000000000000711, -5.000000000000000000, 54.00000000000000711 ) ) ;
#21664 = DIRECTION ( 'NONE',  ( 1.000000000000000000, -1.296372316667914327E-16, 0.000000000000000000 ) ) ;
#21665 = LINE ( 'NONE', #2298, #3377 ) ;
#21666 = EDGE_LOOP ( 'NONE', ( #15229, #22315, #16569 ) ) ;
#21667 = CARTESIAN_POINT ( 'NONE',  ( -42.50000000000000711, -12.00000000000000000, 47.50000000000000711 ) ) ;
#21668 = CARTESIAN_POINT ( 'NONE',  ( -0.8615617109686474206, -36.14854559161353365, -2.932164912090525988 ) ) ;
#21669 = DIRECTION ( 'NONE',  ( 0.000000000000000000, 1.000000000000000000, 0.000000000000000000 ) ) ;
#21670 = ORIENTED_EDGE ( 'NONE', *, *, #21039, .T. ) ;
#21671 = DIRECTION ( 'NONE',  ( -1.296372316667914327E-16, -1.000000000000000000, 0.000000000000000000 ) ) ;
#21672 = FACE_OUTER_BOUND ( 'NONE', #3785, .T. ) ;
#21673 = CARTESIAN_POINT ( 'NONE',  ( -33.99999999999999289, 28.19616000222404040, 0.000000000000000000 ) ) ;
#21674 = ORIENTED_EDGE ( 'NONE', *, *, #10725, .T. ) ;
#21675 = ORIENTED_EDGE ( 'NONE', *, *, #20496, .T. ) ;
#21676 = ORIENTED_EDGE ( 'NONE', *, *, #7110, .T. ) ;
#21677 = DIRECTION ( 'NONE',  ( -0.1990447749484038631, 0.9799897464804870895, 0.001128875037334218937 ) ) ;
#21678 = EDGE_CURVE ( 'NONE', #2902, #2004, #19231, .T. ) ;
#21679 = ORIENTED_EDGE ( 'NONE', *, *, #1766, .T. ) ;
#21680 = CARTESIAN_POINT ( 'NONE',  ( 17.23507576850065348, 30.19164414353179637, 59.89185441256822884 ) ) ;
#21681 = FACE_OUTER_BOUND ( 'NONE', #4185, .T. ) ;
#21682 = VECTOR ( 'NONE', #16495, 1000.000000000000114 ) ;
#21683 = CIRCLE ( 'NONE', #4486, 1.000000000000000888 ) ;
#21684 = CARTESIAN_POINT ( 'NONE',  ( 2.775557561562891351E-14, -2.775557561562891351E-14, 2.999999999999999112 ) ) ;
#21685 = EDGE_CURVE ( 'NONE', #18617, #19759, #9807, .T. ) ;
#21686 = CARTESIAN_POINT ( 'NONE',  ( 6.000000000000000888, -40.00000000000000000, 6.000000000000000000 ) ) ;
#21687 = DIRECTION ( 'NONE',  ( 1.000000000000000000, 0.000000000000000000, 0.000000000000000000 ) ) ;
#21688 = ORIENTED_EDGE ( 'NONE', *, *, #13247, .T. ) ;
#21689 = CARTESIAN_POINT ( 'NONE',  ( -35.00000000000000000, 40.00000000000000000, 1.387778780781445676E-14 ) ) ;
#21690 = LINE ( 'NONE', #17910, #7581 ) ;
#21691 = ORIENTED_EDGE ( 'NONE', *, *, #10026, .F. ) ;
#21692 = CARTESIAN_POINT ( 'NONE',  ( 7.711478842616664942, -31.57187188083537777, 2.999999999999995559 ) ) ;
#21693 = VECTOR ( 'NONE', #6576, 1000.000000000000000 ) ;
#21694 = CARTESIAN_POINT ( 'NONE',  ( -26.79308242454876776, -16.56444186175096078, -2.999999999999971578 ) ) ;
#21695 = CARTESIAN_POINT ( 'NONE',  ( -36.14854559161338443, 0.8615617109687877528, -2.932164912090540199 ) ) ;
#21696 = ORIENTED_EDGE ( 'NONE', *, *, #1151, .F. ) ;
#21697 = CARTESIAN_POINT ( 'NONE',  ( -9.233659704009069102, 40.00000000000000000, -53.41795192421820104 ) ) ;
#21698 = DIRECTION ( 'NONE',  ( 1.000000000000000000, 0.000000000000000000, 1.224646799147352961E-16 ) ) ;
#21699 = EDGE_CURVE ( 'NONE', #15969, #18834, #4322, .T. ) ;
#21700 = VERTEX_POINT ( 'NONE', #2156 ) ;
#21701 = CARTESIAN_POINT ( 'NONE',  ( 7.704812602363275253, 39.66337197165110950, 53.66058689971939089 ) ) ;
#21702 = LINE ( 'NONE', #4405, #5654 ) ;
#21703 = ORIENTED_EDGE ( 'NONE', *, *, #18442, .T. ) ;
#21704 = FACE_OUTER_BOUND ( 'NONE', #2174, .T. ) ;
#21705 = CARTESIAN_POINT ( 'NONE',  ( 16.86064470394643067, 34.83129639055714932, 57.19330778950707384 ) ) ;
#21706 = CARTESIAN_POINT ( 'NONE',  ( -90.00000000000000000, 39.97500000000000142, 2.500000000000001332 ) ) ;
#21707 = AXIS2_PLACEMENT_3D ( 'NONE', #2290, #9282, #16263 ) ;
#21708 = CARTESIAN_POINT ( 'NONE',  ( 15.90155957501127304, 35.87083899979363366, -56.88316157031720621 ) ) ;
#21709 = B_SPLINE_CURVE_WITH_KNOTS ( 'NONE', 3,
 ( #17957, #11188, #539, #2725, #16467, #9243, #2260, #14508 ),
 .UNSPECIFIED., .F., .F.,
 ( 4, 2, 2, 4 ),
 ( 0.000000000000000000, 0.002331395735520895053, 0.004662791471041790106, 0.009325582942083583682 ),
 .UNSPECIFIED. ) ;
#21710 = ORIENTED_EDGE ( 'NONE', *, *, #9179, .T. ) ;
#21711 = EDGE_CURVE ( 'NONE', #675, #21024, #17842, .T. ) ;
#21712 = ORIENTED_EDGE ( 'NONE', *, *, #251, .T. ) ;
#21713 = VERTEX_POINT ( 'NONE', #10726 ) ;
#21714 = ORIENTED_EDGE ( 'NONE', *, *, #15340, .T. ) ;
#21715 = LINE ( 'NONE', #2697, #6687 ) ;
#21716 = CARTESIAN_POINT ( 'NONE',  ( -35.00000000000000000, -9.000000000000001776, 1.387778780781445676E-14 ) ) ;
#21717 = B_SPLINE_CURVE_WITH_KNOTS ( 'NONE', 3,
 ( #3934, #16163, #6098, #11476, #16748, #13174, #14785, #720, #20191, #14893, #4611, #21920, #21680, #9871, #939, #4493, #12953, #16861, #21801, #14676, #13062, #22137, #20421, #18461 ),
 .UNSPECIFIED., .F., .F.,
 ( 4, 2, 2, 2, 2, 2, 2, 2, 2, 2, 2, 4 ),
 ( 0.01913044734024342899, 0.02058416378663299393, 0.02203788023302255886, 0.02494531312580169913, 0.02639902957219127447, 0.02785274601858084981, 0.03076017891135999355, 0.03221389535774956542, 0.03366761180413913035, 0.03657504469691827409, 0.03948247758969741089, 0.04238991048247654769 ),
 .UNSPECIFIED. ) ;
#21718 = VERTEX_POINT ( 'NONE', #17845 ) ;
#21719 = CARTESIAN_POINT ( 'NONE',  ( -16.56444186175071209, 26.79308242454869671, 3.000000000000009770 ) ) ;
#21720 = DIRECTION ( 'NONE',  ( 0.000000000000000000, 0.000000000000000000, 1.000000000000000000 ) ) ;
#21721 = AXIS2_PLACEMENT_3D ( 'NONE', #16441, #7734, #20001 ) ;
#21722 = ORIENTED_EDGE ( 'NONE', *, *, #145, .F. ) ;
#21723 = LINE ( 'NONE', #15391, #3886 ) ;
#21724 = VECTOR ( 'NONE', #17401, 1000.000000000000000 ) ;
#21725 = CARTESIAN_POINT ( 'NONE',  ( 2.670518050928090137, 23.57199239071502817, 8.613211112165400252 ) ) ;
#21726 = CARTESIAN_POINT ( 'NONE',  ( 10.49999999999994316, 42.51666049839543149, -105.0000000000000142 ) ) ;
#21727 = DIRECTION ( 'NONE',  ( -6.505213034913038160E-19, -3.903127820947822896E-18, -1.000000000000000000 ) ) ;
#21728 = CIRCLE ( 'NONE', #9628, 6.499999999999999112 ) ;
#21729 = DIRECTION ( 'NONE',  ( -0.000000000000000000, 1.000000000000000000, -0.000000000000000000 ) ) ;
#21730 = ADVANCED_FACE ( 'NONE', ( #5477 ), #17729, .T. ) ;
#21731 = VECTOR ( 'NONE', #6968, 1000.000000000000000 ) ;
#21732 = CARTESIAN_POINT ( 'NONE',  ( -5.905688108141349701, 39.12130528552482644, 53.51375100093226678 ) ) ;
#21733 = CARTESIAN_POINT ( 'NONE',  ( 35.00000000000000000, 40.00000000000000000, 4.258610482196280173E-15 ) ) ;
#21734 = ORIENTED_EDGE ( 'NONE', *, *, #17048, .F. ) ;
#21735 = EDGE_CURVE ( 'NONE', #5940, #1508, #3929, .T. ) ;
#21736 = EDGE_CURVE ( 'NONE', #2079, #8181, #16001, .T. ) ;
#21737 = CIRCLE ( 'NONE', #7086, 2.500000000000002220 ) ;
#21738 = ORIENTED_EDGE ( 'NONE', *, *, #4105, .F. ) ;
#21739 = AXIS2_PLACEMENT_3D ( 'NONE', #16481, #15396, #5835 ) ;
#21740 = CIRCLE ( 'NONE', #8201, 2.500000000000002220 ) ;
#21741 = ORIENTED_EDGE ( 'NONE', *, *, #7897, .T. ) ;
#21742 = DIRECTION ( 'NONE',  ( -0.000000000000000000, 1.000000000000000000, -0.000000000000000000 ) ) ;
#21743 = CARTESIAN_POINT ( 'NONE',  ( -35.00000000000058265, 40.00000000000000711, -52.47500000000076170 ) ) ;
#21744 = EDGE_CURVE ( 'NONE', #18308, #1985, #21178, .T. ) ;
#21745 = AXIS2_PLACEMENT_3D ( 'NONE', #13763, #441, #20779 ) ;
#21746 = DIRECTION ( 'NONE',  ( -0.000000000000000000, 1.000000000000000000, -0.000000000000000000 ) ) ;
#21747 = DIRECTION ( 'NONE',  ( 6.505213034913038160E-19, 3.903127820947822896E-18, 1.000000000000000000 ) ) ;
#21748 = CARTESIAN_POINT ( 'NONE',  ( 7.325260514639500961E-15, -4.648749848371387827, 45.43309249825157536 ) ) ;
#21749 = LINE ( 'NONE', #6046, #20356 ) ;
#21750 = LINE ( 'NONE', #889, #13703 ) ;
#21751 = CARTESIAN_POINT ( 'NONE',  ( 11.35354668330729133, 30.33632613426176405, -2.999999999999978240 ) ) ;
#21752 = PRODUCT_DEFINITION_SHAPE ( 'NONE', 'NONE',  #22704 ) ;
#21753 = AXIS2_PLACEMENT_3D ( 'NONE', #21886, #6185, #10990 ) ;
#21754 = ORIENTED_EDGE ( 'NONE', *, *, #13220, .T. ) ;
#21755 = DIRECTION ( 'NONE',  ( 0.000000000000000000, 0.000000000000000000, -1.000000000000000000 ) ) ;
#21756 = FACE_OUTER_BOUND ( 'NONE', #14092, .T. ) ;
#21757 = DIRECTION ( 'NONE',  ( -6.505213034913038160E-19, -3.903127820947822896E-18, -1.000000000000000000 ) ) ;
#21758 = EDGE_CURVE ( 'NONE', #7391, #22536, #16004, .T. ) ;
#21759 = DIRECTION ( 'NONE',  ( -1.000000000000000000, -1.208970125616060717E-17, 0.000000000000000000 ) ) ;
#21760 = AXIS2_PLACEMENT_3D ( 'NONE', #17175, #18789, #22585 ) ;
#21761 = ORIENTED_EDGE ( 'NONE', *, *, #7813, .F. ) ;
#21762 = DIRECTION ( 'NONE',  ( -0.000000000000000000, 1.000000000000000000, -0.000000000000000000 ) ) ;
#21763 = ORIENTED_EDGE ( 'NONE', *, *, #10185, .F. ) ;
#21764 = DIRECTION ( 'NONE',  ( 1.000000000000000000, 1.208970125616063028E-17, 0.000000000000000000 ) ) ;
#21765 = DIRECTION ( 'NONE',  ( -1.000000000000000000, 1.530638361156006245E-16, 0.000000000000000000 ) ) ;
#21766 = AXIS2_PLACEMENT_3D ( 'NONE', #6178, #6620, #6397 ) ;
#21767 = EDGE_LOOP ( 'NONE', ( #3083, #8102, #246, #9224 ) ) ;
#21768 = AXIS2_PLACEMENT_3D ( 'NONE', #183, #21054, #1698 ) ;
#21769 = CARTESIAN_POINT ( 'NONE',  ( 33.47097213929444592, -11.93830856187230971, 3.000000000000051514 ) ) ;
#21770 = CARTESIAN_POINT ( 'NONE',  ( 1.582593789249429506, 40.00000000000000000, -49.73343818203412070 ) ) ;
#21771 = ORIENTED_EDGE ( 'NONE', *, *, #8351, .T. ) ;
#21772 = CARTESIAN_POINT ( 'NONE',  ( 9.689843208404422370, 39.33333333333334281, -54.54983754392748097 ) ) ;
#21773 = CARTESIAN_POINT ( 'NONE',  ( 11.49398617736656014, 40.00000000000000711, 54.13866599136176916 ) ) ;
#21774 = ADVANCED_FACE ( 'NONE', ( #317 ), #8805, .F. ) ;
#21775 = CARTESIAN_POINT ( 'NONE',  ( 0.000000000000000000, 28.49999999999998934, 0.000000000000000000 ) ) ;
#21776 = CARTESIAN_POINT ( 'NONE',  ( 10.27431133777637484, -4.928932188134504955, -51.43682631505696179 ) ) ;
#21777 = CIRCLE ( 'NONE', #17018, 19.11328065563150957 ) ;
#21778 = CARTESIAN_POINT ( 'NONE',  ( -14.70622169670557078, 6.333487747695555115, -56.50111465619737317 ) ) ;
#21779 = CYLINDRICAL_SURFACE ( 'NONE', #19584, 19.11328065563150957 ) ;
#21780 = DIRECTION ( 'NONE',  ( 0.000000000000000000, 0.000000000000000000, 1.000000000000000000 ) ) ;
#21781 = ORIENTED_EDGE ( 'NONE', *, *, #22362, .T. ) ;
#21782 = DIRECTION ( 'NONE',  ( 0.000000000000000000, 0.7071067811865352493, 0.7071067811865597852 ) ) ;
#21783 = TOROIDAL_SURFACE ( 'NONE', #12560, 34.90673715956759082, 8.750000000000000000 ) ;
#21784 = PLANE ( 'NONE',  #16244 ) ;
#21785 = ADVANCED_FACE ( 'NONE', ( #14387 ), #17102, .T. ) ;
#21786 = EDGE_CURVE ( 'NONE', #507, #164, #12711, .T. ) ;
#21787 = CYLINDRICAL_SURFACE ( 'NONE', #12210, 15.00000000000000000 ) ;
#21788 = ADVANCED_FACE ( 'NONE', ( #10843 ), #14042, .F. ) ;
#21789 = AXIS2_PLACEMENT_3D ( 'NONE', #17201, #17088, #13410 ) ;
#21790 = ORIENTED_EDGE ( 'NONE', *, *, #14205, .T. ) ;
#21791 = CARTESIAN_POINT ( 'NONE',  ( -5.833333333333328596, 33.81926995981417861, 40.61164310337068173 ) ) ;
#21792 = DIRECTION ( 'NONE',  ( 0.000000000000000000, 0.000000000000000000, 1.000000000000000000 ) ) ;
#21793 = EDGE_CURVE ( 'NONE', #17279, #4267, #21709, .T. ) ;
#21794 = CIRCLE ( 'NONE', #3133, 34.90673715956759082 ) ;
#21795 = ORIENTED_EDGE ( 'NONE', *, *, #12837, .T. ) ;
#21796 = AXIS2_PLACEMENT_3D ( 'NONE', #1930, #17735, #2042 ) ;
#21797 = ORIENTED_EDGE ( 'NONE', *, *, #21889, .F. ) ;
#21798 = CIRCLE ( 'NONE', #15975, 1.000000000000000888 ) ;
#21799 = DIRECTION ( 'NONE',  ( -0.3494467096846017862, 0.9369561036350800842, 0.0005069039110796120986 ) ) ;
#21800 = VERTEX_POINT ( 'NONE', #773 ) ;
#21801 = CARTESIAN_POINT ( 'NONE',  ( 13.65693838750919120, 34.64075751992691465, 58.69913499740202667 ) ) ;
#21802 = AXIS2_PLACEMENT_3D ( 'NONE', #13747, #6905, #13967 ) ;
#21803 = CARTESIAN_POINT ( 'NONE',  ( 4.842578813362819368, -0.8535550256951374148, 51.47191290771596783 ) ) ;
#21804 = CARTESIAN_POINT ( 'NONE',  ( -1.568459684872854920, 24.67391323484813626, 8.880481854261104147 ) ) ;
#21805 = FACE_OUTER_BOUND ( 'NONE', #13580, .T. ) ;
#21806 = ADVANCED_FACE ( 'NONE', ( #18185, #881 ), #14840, .F. ) ;
#21807 = FACE_OUTER_BOUND ( 'NONE', #4259, .T. ) ;
#21808 = ORIENTED_EDGE ( 'NONE', *, *, #17996, .T. ) ;
#21809 = DIRECTION ( 'NONE',  ( 6.505213034913038160E-19, 3.903127820947822896E-18, 1.000000000000000000 ) ) ;
#21810 = CARTESIAN_POINT ( 'NONE',  ( -12.99999999999980282, -2.516660498395516310, 105.0000000000000142 ) ) ;
#21811 = EDGE_LOOP ( 'NONE', ( #14288, #13190, #1345, #5911 ) ) ;
#21812 = CARTESIAN_POINT ( 'NONE',  ( -13.59841332577231832, 13.65742718326612604, -45.18857684126742669 ) ) ;
#21813 = CARTESIAN_POINT ( 'NONE',  ( 9.594672135725315573E-15, 39.99999999999997158, 48.73397172404484223 ) ) ;
#21814 = ORIENTED_EDGE ( 'NONE', *, *, #3782, .T. ) ;
#21815 = CYLINDRICAL_SURFACE ( 'NONE', #4724, 8.999999999999998224 ) ;
#21816 = VERTEX_POINT ( 'NONE', #10964 ) ;
#21817 = CARTESIAN_POINT ( 'NONE',  ( 0.7060532431912704965, 40.00000000000297717, 49.41655072425569983 ) ) ;
#21818 = VECTOR ( 'NONE', #18755, 1000.000000000000000 ) ;
#21819 = CARTESIAN_POINT ( 'NONE',  ( 1.387778780781445676E-14, -3.999999999999985345, -48.73397172404115452 ) ) ;
#21820 = CARTESIAN_POINT ( 'NONE',  ( -7.864084088052238365E-15, -0.02545116923825692726, -50.05029972084987122 ) ) ;
#21821 = CIRCLE ( 'NONE', #17035, 36.76383501243555685 ) ;
#21822 = ADVANCED_FACE ( 'NONE', ( #11419 ), #2499, .T. ) ;
#21823 = AXIS2_PLACEMENT_3D ( 'NONE', #14940, #1101, #6145 ) ;
#21824 = EDGE_LOOP ( 'NONE', ( #10538, #11698, #11596, #21035 ) ) ;
#21825 = CARTESIAN_POINT ( 'NONE',  ( 21.41958700883258970, 27.56232195404059837, 3.000000000000002665 ) ) ;
#21826 = DIRECTION ( 'NONE',  ( 6.505213034913038160E-19, 3.903127820947822896E-18, 1.000000000000000000 ) ) ;
#21827 = EDGE_CURVE ( 'NONE', #5630, #11767, #2378, .T. ) ;
#21828 = AXIS2_PLACEMENT_3D ( 'NONE', #17633, #335, #3779 ) ;
#21829 = EDGE_CURVE ( 'NONE', #5003, #20565, #16746, .T. ) ;
#21830 = FACE_BOUND ( 'NONE', #16410, .T. ) ;
#21831 = ORIENTED_EDGE ( 'NONE', *, *, #688, .T. ) ;
#21832 = ORIENTED_EDGE ( 'NONE', *, *, #11528, .F. ) ;
#21833 = EDGE_CURVE ( 'NONE', #15580, #2477, #14621, .T. ) ;
#21834 = ORIENTED_EDGE ( 'NONE', *, *, #17946, .F. ) ;
#21835 = CIRCLE ( 'NONE', #6829, 39.00000000000001421 ) ;
#21836 = AXIS2_PLACEMENT_3D ( 'NONE', #18066, #4337, #18530 ) ;
#21837 = CIRCLE ( 'NONE', #6466, 19.11328065563152379 ) ;
#21838 = ORIENTED_EDGE ( 'NONE', *, *, #8801, .F. ) ;
#21839 = DIRECTION ( 'NONE',  ( -1.000000000000000000, -1.208970125616077665E-17, 0.000000000000000000 ) ) ;
#21840 = CARTESIAN_POINT ( 'NONE',  ( -34.99999999999999289, 40.00000000000000000, 58.99999999999995737 ) ) ;
#21841 = AXIS2_PLACEMENT_3D ( 'NONE', #6989, #9037, #13945 ) ;
#21842 = VERTEX_POINT ( 'NONE', #13006 ) ;
#21843 = CARTESIAN_POINT ( 'NONE',  ( 11.68090480754630178, 3.765577839755386069, 57.90797000640142045 ) ) ;
#21844 = DIRECTION ( 'NONE',  ( 0.000000000000000000, 0.000000000000000000, 1.000000000000000000 ) ) ;
#21845 = ORIENTED_EDGE ( 'NONE', *, *, #19705, .F. ) ;
#21846 = AXIS2_PLACEMENT_3D ( 'NONE', #2255, #14266, #16220 ) ;
#21847 = ORIENTED_EDGE ( 'NONE', *, *, #9711, .T. ) ;
#21848 = DIRECTION ( 'NONE',  ( -6.505213034913038160E-19, -3.903127820947822896E-18, -1.000000000000000000 ) ) ;
#21849 = LINE ( 'NONE', #7977, #19346 ) ;
#21850 = CARTESIAN_POINT ( 'NONE',  ( -12.31876324338268525, -30.07487443287973505, 2.999999999999995559 ) ) ;
#21851 = CARTESIAN_POINT ( 'NONE',  ( -0.4054897353551412120, 39.99903132614927159, 49.04700738630989321 ) ) ;
#21852 = AXIS2_PLACEMENT_3D ( 'NONE', #4818, #13384, #16848 ) ;
#21853 = EDGE_CURVE ( 'NONE', #19371, #19744, #10520, .T. ) ;
#21854 = CARTESIAN_POINT ( 'NONE',  ( -0.7832310603219697631, 40.00000000000097344, 49.34583618815681660 ) ) ;
#21855 = CARTESIAN_POINT ( 'NONE',  ( 3.849727973822423851E-15, 1.500000000000011768, 0.000000000000000000 ) ) ;
#21856 = EDGE_LOOP ( 'NONE', ( #2625, #13054, #20325, #8787 ) ) ;
#21857 = CONICAL_SURFACE ( 'NONE', #16311, 2.524999999999999467, 0.7853981633974482790 ) ;
#21858 = VERTEX_POINT ( 'NONE', #21631 ) ;
#21859 = ORIENTED_EDGE ( 'NONE', *, *, #357, .F. ) ;
#21860 = CARTESIAN_POINT ( 'NONE',  ( -17.96553007763869658, 11.19640018278690263, 57.57421575614280584 ) ) ;
#21861 = CARTESIAN_POINT ( 'NONE',  ( -1.039655021832667670, -3.147609295952975561, -46.52691668518789214 ) ) ;
#21862 = CARTESIAN_POINT ( 'NONE',  ( -89.99999999999701572, -5.000000000000000000, -3.012171160963566127E-14 ) ) ;
#21863 = CARTESIAN_POINT ( 'NONE',  ( 0.6844983420876992186, -1.267142481712868474, -48.72692999688269566 ) ) ;
#21864 = AXIS2_PLACEMENT_3D ( 'NONE', #1584, #4915, #15088 ) ;
#21865 = EDGE_CURVE ( 'NONE', #14190, #12296, #4333, .T. ) ;
#21866 = DIRECTION ( 'NONE',  ( 1.000000000000000000, 0.000000000000000000, 0.000000000000000000 ) ) ;
#21867 = CARTESIAN_POINT ( 'NONE',  ( -5.833333333333339255, 40.00000000000000000, -40.61164310337066041 ) ) ;
#21868 = CARTESIAN_POINT ( 'NONE',  ( -35.00000000000000000, 25.00000000000000000, 2.365113165210053967E-14 ) ) ;
#21869 = CARTESIAN_POINT ( 'NONE',  ( -6.433485051969688229, 38.94088993357593154, -55.16018527339667088 ) ) ;
#21870 = DIRECTION ( 'NONE',  ( -1.000000000000000000, -1.208970125616063182E-17, 0.000000000000000000 ) ) ;
#21871 = ADVANCED_FACE ( 'NONE', ( #18299, #5818 ), #7995, .F. ) ;
#21872 = ORIENTED_EDGE ( 'NONE', *, *, #21328, .F. ) ;
#21873 = AXIS2_PLACEMENT_3D ( 'NONE', #1846, #14187, #15798 ) ;
#21874 = DIRECTION ( 'NONE',  ( -0.000000000000000000, -1.000000000000000000, -0.000000000000000000 ) ) ;
#21875 = CARTESIAN_POINT ( 'NONE',  ( 15.49999999999993960, 42.51666049839543149, 105.0000000000000142 ) ) ;
#21876 = CARTESIAN_POINT ( 'NONE',  ( 16.23901130406737181, 8.288052467682684110, 57.02826995000636146 ) ) ;
#21877 = DIRECTION ( 'NONE',  ( -0.000000000000000000, 1.000000000000000000, -0.000000000000000000 ) ) ;
#21878 = ORIENTED_EDGE ( 'NONE', *, *, #17742, .F. ) ;
#21879 = CARTESIAN_POINT ( 'NONE',  ( -1.387778780781445676E-14, 40.00000000000000000, -48.73397172404481381 ) ) ;
#21880 = CYLINDRICAL_SURFACE ( 'NONE', #21766, 1.000000000000000888 ) ;
#21881 = CARTESIAN_POINT ( 'NONE',  ( 30.13956425491254265, 21.05198877411773495, 2.800654218530485018 ) ) ;
#21882 = CIRCLE ( 'NONE', #13803, 2.500000000000008882 ) ;
#21883 = DIRECTION ( 'NONE',  ( 1.296372316667914327E-16, 1.000000000000000000, -0.000000000000000000 ) ) ;
#21884 = CIRCLE ( 'NONE', #10144, 1.000000000000000888 ) ;
#21885 = ORIENTED_EDGE ( 'NONE', *, *, #10376, .T. ) ;
#21886 = CARTESIAN_POINT ( 'NONE',  ( -13.00000000000011546, 42.51666049839536043, 100.0000000000000000 ) ) ;
#21887 = AXIS2_PLACEMENT_3D ( 'NONE', #18544, #15078, #2967 ) ;
#21888 = CARTESIAN_POINT ( 'NONE',  ( -32.14641817400170964, -18.83615802559815577, -2.999999999999971578 ) ) ;
#21889 = EDGE_CURVE ( 'NONE', #12492, #17781, #21884, .T. ) ;
#21890 = ORIENTED_EDGE ( 'NONE', *, *, #21082, .T. ) ;
#21891 = CARTESIAN_POINT ( 'NONE',  ( -0.003185071962412873176, 13.00000169078104051, 8.999999436406458386 ) ) ;
#21892 = AXIS2_PLACEMENT_3D ( 'NONE', #13256, #13377, #6192 ) ;
#21893 = CARTESIAN_POINT ( 'NONE',  ( 10.43027093729392618, 39.22757009021464114, 54.80615623442351847 ) ) ;
#21894 = AXIS2_PLACEMENT_3D ( 'NONE', #16100, #10708, #10487 ) ;
#21895 = DIRECTION ( 'NONE',  ( -0.000000000000000000, 1.000000000000000000, -0.000000000000000000 ) ) ;
#21896 = B_SPLINE_CURVE_WITH_KNOTS ( 'NONE', 3,
 ( #1992, #3617, #17803, #3384, #13782, #6937, #10461, #7144, #12086, #22523, #12189, #20798 ),
 .UNSPECIFIED., .F., .F.,
 ( 4, 2, 2, 2, 2, 4 ),
 ( 0.006347202264228477345, 0.007930096811551049646, 0.008721544085212338399, 0.009512991358873625417, 0.01109588590619620292, 0.01267878045351878216 ),
 .UNSPECIFIED. ) ;
#21897 = CARTESIAN_POINT ( 'NONE',  ( -2.734690830816374874, 39.99999999999998579, 50.39884290491228569 ) ) ;
#21898 = DIRECTION ( 'NONE',  ( -0.000000000000000000, -1.000000000000000000, -0.000000000000000000 ) ) ;
#21899 = CARTESIAN_POINT ( 'NONE',  ( -9.454382208758131512, 39.37264146017265176, 54.46710161869616940 ) ) ;
#21900 = ADVANCED_FACE ( 'NONE', ( #4102 ), #7873, .F. ) ;
#21901 = DIRECTION ( 'NONE',  ( 0.000000000000000000, 0.000000000000000000, 1.000000000000000000 ) ) ;
#21902 = ORIENTED_EDGE ( 'NONE', *, *, #18741, .T. ) ;
#21903 = FACE_OUTER_BOUND ( 'NONE', #9675, .T. ) ;
#21904 = FACE_OUTER_BOUND ( 'NONE', #15512, .T. ) ;
#21905 = CARTESIAN_POINT ( 'NONE',  ( -0.03494506074407652957, 39.99999280907451293, -48.76115732596038299 ) ) ;
#21906 = VERTEX_POINT ( 'NONE', #5926 ) ;
#21907 = VECTOR ( 'NONE', #10072, 1000.000000000000000 ) ;
#21908 = CARTESIAN_POINT ( 'NONE',  ( -14.94062893683336668, 21.54390686295445079, 45.79998742252197275 ) ) ;
#21909 = DIRECTION ( 'NONE',  ( -0.000000000000000000, -1.000000000000000000, -0.000000000000000000 ) ) ;
#21910 = AXIS2_PLACEMENT_3D ( 'NONE', #22300, #18627, #6250 ) ;
#21911 = AXIS2_PLACEMENT_3D ( 'NONE', #20914, #21023, #1779 ) ;
#21912 = ADVANCED_FACE ( 'NONE', ( #19691 ), #13128, .F. ) ;
#21913 = VECTOR ( 'NONE', #7561, 1000.000000000000114 ) ;
#21914 = ORIENTED_EDGE ( 'NONE', *, *, #17370, .F. ) ;
#21915 = ORIENTED_EDGE ( 'NONE', *, *, #22285, .F. ) ;
#21916 = DIRECTION ( 'NONE',  ( 0.3494467096846017862, -0.9369561036350800842, -0.0005069039110796164354 ) ) ;
#21917 = EDGE_CURVE ( 'NONE', #15452, #13636, #5781, .T. ) ;
#21918 = ADVANCED_FACE ( 'NONE', ( #16350 ), #7652, .T. ) ;
#21919 = ORIENTED_EDGE ( 'NONE', *, *, #22501, .F. ) ;
#21920 = CARTESIAN_POINT ( 'NONE',  ( 17.70396115872092935, 29.35428329955200866, 60.02641142872583657 ) ) ;
#21921 = DIRECTION ( 'NONE',  ( 8.659560562354844111E-17, 0.7071067811865549002, -0.7071067811865402453 ) ) ;
#21922 = CARTESIAN_POINT ( 'NONE',  ( -2.999999999999998668, 22.00000000000000355, 8.485281374238567764 ) ) ;
#21923 = CYLINDRICAL_SURFACE ( 'NONE', #9441, 2.499999999999998668 ) ;
#21924 = DIRECTION ( 'NONE',  ( -6.505213034913038160E-19, -3.903127820947822896E-18, -1.000000000000000000 ) ) ;
#21925 = ORIENTED_EDGE ( 'NONE', *, *, #4723, .F. ) ;
#21926 = DIRECTION ( 'NONE',  ( -0.000000000000000000, 1.000000000000000000, -0.000000000000000000 ) ) ;
#21928 = CIRCLE ( 'NONE', #13117, 18.00000000000000000 ) ;
#21927 = CYLINDRICAL_SURFACE ( 'NONE', #4670, 36.76383501243555685 ) ;
#21929 = ORIENTED_EDGE ( 'NONE', *, *, #12037, .T. ) ;
#21930 = DIRECTION ( 'NONE',  ( -0.000000000000000000, 1.000000000000000000, -0.000000000000000000 ) ) ;
#21931 = CARTESIAN_POINT ( 'NONE',  ( -19.47136665037378833, 8.793048248091416497, -57.95785196855348431 ) ) ;
#21932 = FACE_OUTER_BOUND ( 'NONE', #1403, .T. ) ;
#21933 = ORIENTED_EDGE ( 'NONE', *, *, #16695, .F. ) ;
#21934 = CARTESIAN_POINT ( 'NONE',  ( -2.422192751863727622, -32.40961249803553557, 3.000000000000023537 ) ) ;
#21935 = CARTESIAN_POINT ( 'NONE',  ( 6.401811138932578693, 38.95166772950821610, -55.13648753466789287 ) ) ;
#21936 = ORIENTED_EDGE ( 'NONE', *, *, #14863, .T. ) ;
#21937 = CARTESIAN_POINT ( 'NONE',  ( 7.555723902516218615, 38.52224445567402711, 55.93227658743226272 ) ) ;
#21938 = EDGE_CURVE ( 'NONE', #3991, #3967, #11756, .T. ) ;
#21939 = DIRECTION ( 'NONE',  ( -0.000000000000000000, 1.000000000000000000, -0.000000000000000000 ) ) ;
#21940 = CARTESIAN_POINT ( 'NONE',  ( -0.3713120412951391169, -0.009378283650370923194, -50.78681545405707709 ) ) ;
#21941 = VERTEX_POINT ( 'NONE', #15299 ) ;
#21942 = DIRECTION ( 'NONE',  ( 0.000000000000000000, -1.000000000000000000, 0.000000000000000000 ) ) ;
#21943 = CARTESIAN_POINT ( 'NONE',  ( 9.165377225651162973, 37.79989650906291132, 54.16098472236621575 ) ) ;
#21944 = CARTESIAN_POINT ( 'NONE',  ( -9.999999999999758415, -3.000000000000169198, -4.999999999999984013 ) ) ;
#21945 = ADVANCED_FACE ( 'NONE', ( #20698 ), #10142, .T. ) ;
#21946 = CARTESIAN_POINT ( 'NONE',  ( 18.09042992579335163, 28.57522027848957080, -57.61279183054943331 ) ) ;
#21947 = ADVANCED_FACE ( 'NONE', ( #8105 ), #15407, .T. ) ;
#21948 = CIRCLE ( 'NONE', #4736, 1.000000000000001776 ) ;
#21949 = VERTEX_POINT ( 'NONE', #9821 ) ;
#21950 = ORIENTED_EDGE ( 'NONE', *, *, #5275, .F. ) ;
#21951 = ORIENTED_EDGE ( 'NONE', *, *, #16317, .F. ) ;
#21952 = ADVANCED_FACE ( 'NONE', ( #5010 ), #21532, .F. ) ;
#21953 = ORIENTED_EDGE ( 'NONE', *, *, #15400, .T. ) ;
#21954 = CARTESIAN_POINT ( 'NONE',  ( 2.999929132934961995, 22.39707156654313991, 6.485306429529692274 ) ) ;
#21955 = PRODUCT_DEFINITION_SHAPE ( 'NONE', 'NONE',  #7439 ) ;
#21956 = CARTESIAN_POINT ( 'NONE',  ( 34.99999999999999289, -5.000000000000000000, -52.49999999999705835 ) ) ;
#21957 = ORIENTED_EDGE ( 'NONE', *, *, #4553, .F. ) ;
#21958 = CARTESIAN_POINT ( 'NONE',  ( 10.99584631063691909, 3.272668205460111945, 57.61971594758629323 ) ) ;
#21959 = DIRECTION ( 'NONE',  ( 1.000000000000000000, 1.208970125616063182E-17, 0.000000000000000000 ) ) ;
#21960 = EDGE_LOOP ( 'NONE', ( #10022, #2337, #5694, #4748, #10586 ) ) ;
#21961 = DIRECTION ( 'NONE',  ( 1.000000000000000000, -7.981516076044952263E-15, 0.000000000000000000 ) ) ;
#21962 = EDGE_CURVE ( 'NONE', #5560, #22077, #18973, .T. ) ;
#21963 = AXIS2_PLACEMENT_3D ( 'NONE', #11325, #16479, #10979 ) ;
#21964 = EDGE_LOOP ( 'NONE', ( #2865, #4171, #8409, #2608, #9169, #1267 ) ) ;
#21965 = CARTESIAN_POINT ( 'NONE',  ( 15.50000000000024336, -2.516660498395250745, 100.0000000000000000 ) ) ;
#21966 = EDGE_CURVE ( 'NONE', #5340, #15747, #15661, .T. ) ;
#21967 = CARTESIAN_POINT ( 'NONE',  ( 0.003185071962414435728, 24.99999830921895594, 8.999999436406460163 ) ) ;
#21968 = CARTESIAN_POINT ( 'NONE',  ( 35.00000000000058265, 28.00000000000000000, -55.00000000000076028 ) ) ;
#21969 = CARTESIAN_POINT ( 'NONE',  ( -0.1964574450121475135, 39.99977788120574473, 48.88630899457443491 ) ) ;
#21970 = EDGE_CURVE ( 'NONE', #3030, #7098, #9468, .T. ) ;
#21971 = AXIS2_PLACEMENT_3D ( 'NONE', #6659, #3459, #20636 ) ;
#21972 = CARTESIAN_POINT ( 'NONE',  ( -11.13407802442741534, 9.941921282207673016, 43.93745127716451293 ) ) ;
#21973 = DIRECTION ( 'NONE',  ( -6.505213034913038160E-19, -3.903127820947822896E-18, -1.000000000000000000 ) ) ;
#21974 = ORIENTED_EDGE ( 'NONE', *, *, #9755, .T. ) ;
#21975 = ORIENTED_EDGE ( 'NONE', *, *, #12527, .F. ) ;
#21976 = CIRCLE ( 'NONE', #14251, 2.500000000000002220 ) ;
#21977 = ORIENTED_EDGE ( 'NONE', *, *, #12978, .T. ) ;
#21978 = CARTESIAN_POINT ( 'NONE',  ( -17.11943327291902150, 30.37830191768460963, 59.85657255524080966 ) ) ;
#21979 = CARTESIAN_POINT ( 'NONE',  ( 34.74700806321118307, -12.00937115242659026, -2.000000000000001776 ) ) ;
#21980 = CARTESIAN_POINT ( 'NONE',  ( 37.10000000000058407, 28.00000000000000000, -55.00000000000076028 ) ) ;
#21981 = EDGE_CURVE ( 'NONE', #3437, #19781, #9817, .T. ) ;
#21982 = VECTOR ( 'NONE', #22453, 1000.000000000000000 ) ;
#21983 = CARTESIAN_POINT ( 'NONE',  ( 35.00000000000000000, 0.000000000000000000, -9.000000000000000000 ) ) ;
#21984 = CARTESIAN_POINT ( 'NONE',  ( 0.6237373291636730821, 39.99088417130652573, 49.47180386667442775 ) ) ;
#21985 = LINE ( 'NONE', #20257, #17871 ) ;
#21986 = CARTESIAN_POINT ( 'NONE',  ( -6.297060429293823702, 38.99690089842329854, -53.73986014815309886 ) ) ;
#21987 = CARTESIAN_POINT ( 'NONE',  ( 42.49999999999998579, 10.00000000000000000, -47.49999999999997868 ) ) ;
#21988 = ORIENTED_EDGE ( 'NONE', *, *, #4592, .T. ) ;
#21989 = EDGE_CURVE ( 'NONE', #2304, #5844, #16914, .T. ) ;
#21990 = CARTESIAN_POINT ( 'NONE',  ( -10.64189282879911147, 39.19489805854265541, 54.88474174651651794 ) ) ;
#21991 = CYLINDRICAL_SURFACE ( 'NONE', #15897, 60.00000000000000000 ) ;
#21992 = CARTESIAN_POINT ( 'NONE',  ( 3.330669073875469621E-13, -1.110223024625156540E-13, -2.999999999999971578 ) ) ;
#21993 = ORIENTED_EDGE ( 'NONE', *, *, #11404, .F. ) ;
#21994 = ORIENTED_EDGE ( 'NONE', *, *, #13506, .T. ) ;
#21995 = CARTESIAN_POINT ( 'NONE',  ( -35.00000000000000000, 25.00000000000000000, 9.000000000000015987 ) ) ;
#21996 = CYLINDRICAL_SURFACE ( 'NONE', #20366, 19.11328065563152379 ) ;
#21997 = AXIS2_PLACEMENT_3D ( 'NONE', #5907, #16443, #753 ) ;
#21998 = DIRECTION ( 'NONE',  ( -1.000000000000000000, -1.208970125616044077E-17, 0.000000000000000000 ) ) ;
#21999 = ADVANCED_FACE ( 'NONE', ( #13570 ), #4672, .T. ) ;
#22000 = CARTESIAN_POINT ( 'NONE',  ( 8.640968485947571054, 40.00000000000000000, -53.20846482585461246 ) ) ;
#22001 = ORIENTED_EDGE ( 'NONE', *, *, #21981, .F. ) ;
#22002 = DIRECTION ( 'NONE',  ( -0.000000000000000000, 1.000000000000000000, -0.000000000000000000 ) ) ;
#22003 = DIRECTION ( 'NONE',  ( 6.505213034913038160E-19, 3.903127820947822896E-18, 1.000000000000000000 ) ) ;
#22004 = DIRECTION ( 'NONE',  ( -0.000000000000000000, 1.000000000000000000, -0.000000000000000000 ) ) ;
#22005 = CARTESIAN_POINT ( 'NONE',  ( 2.775557561562891351E-14, -2.775557561562891351E-14, 2.999999999999999112 ) ) ;
#22006 = CARTESIAN_POINT ( 'NONE',  ( -9.579024991656989840, 31.54842267267897427, -43.05667825653219438 ) ) ;
#22007 = LINE ( 'NONE', #11455, #74 ) ;
#22008 = EDGE_LOOP ( 'NONE', ( #10041, #10992, #11000, #509, #10796, #20642 ) ) ;
#22009 = CARTESIAN_POINT ( 'NONE',  ( 25.00000000000000355, 20.00000000000000000, 16.49999999999999289 ) ) ;
#22010 = FACE_OUTER_BOUND ( 'NONE', #5550, .T. ) ;
#22011 = CARTESIAN_POINT ( 'NONE',  ( 8.349099696861287612, 1.803277857259548034, -53.93591755799870668 ) ) ;
#22012 = DIRECTION ( 'NONE',  ( -0.000000000000000000, 1.000000000000000000, -0.000000000000000000 ) ) ;
#22013 = ORIENTED_EDGE ( 'NONE', *, *, #11273, .T. ) ;
#22014 = CARTESIAN_POINT ( 'NONE',  ( 3.849727973822423851E-15, 1.500000000000011768, 0.000000000000000000 ) ) ;
#22015 = DIRECTION ( 'NONE',  ( -6.505213034913038160E-19, -3.903127820947822896E-18, -1.000000000000000000 ) ) ;
#22016 = EDGE_CURVE ( 'NONE', #2374, #11218, #13088, .T. ) ;
#22017 = AXIS2_PLACEMENT_3D ( 'NONE', #5604, #5499, #14417 ) ;
#22018 = CIRCLE ( 'NONE', #15401, 34.90673715956759082 ) ;
#22019 = PRODUCT_DEFINITION ( 'UNKNOWN', '', #15689, #12542 ) ;
#22020 = ORIENTED_EDGE ( 'NONE', *, *, #3031, .T. ) ;
#22021 = ADVANCED_FACE ( 'NONE', ( #4893 ), #16810, .F. ) ;
#22022 = ORIENTED_EDGE ( 'NONE', *, *, #21508, .F. ) ;
#22023 = ORIENTED_EDGE ( 'NONE', *, *, #1400, .F. ) ;
#22024 = CARTESIAN_POINT ( 'NONE',  ( 13.63965147459808946, 34.63504322468456564, -58.68815147418791867 ) ) ;
#22025 = DIRECTION ( 'NONE',  ( 0.000000000000000000, -1.000000000000000000, 0.000000000000000000 ) ) ;
#22026 = DIRECTION ( 'NONE',  ( 6.505213034913038160E-19, 3.903127820947822896E-18, 1.000000000000000000 ) ) ;
#22027 = CARTESIAN_POINT ( 'NONE',  ( 15.34286839272954950, 7.164559734098753019, 59.29291272740924512 ) ) ;
#22028 = CARTESIAN_POINT ( 'NONE',  ( 5.422195817667230244, 6.007182364969045452, -40.31637036980818323 ) ) ;
#22029 = ORIENTED_EDGE ( 'NONE', *, *, #12441, .T. ) ;
#22030 = DIRECTION ( 'NONE',  ( -1.296372316667914327E-16, -1.000000000000000000, 0.000000000000000000 ) ) ;
#22031 = DIRECTION ( 'NONE',  ( 8.659560562354902043E-17, -0.7071067811865500152, 0.7071067811865450192 ) ) ;
#22032 = EDGE_LOOP ( 'NONE', ( #3332, #6516, #17645, #3659, #10919 ) ) ;
#22033 = CARTESIAN_POINT ( 'NONE',  ( -14.52224280010138102, 16.16745304956414842, -45.61498238574513664 ) ) ;
#22034 = CARTESIAN_POINT ( 'NONE',  ( 16.66666666666666430, 20.00000000000000000, 23.57022603955159212 ) ) ;
#22035 = CARTESIAN_POINT ( 'NONE',  ( 22.15900668633799597, 29.33526866242080899, -2.800654218530477912 ) ) ;
#22036 = CARTESIAN_POINT ( 'NONE',  ( 18.48876241336177983, 12.20729522219678920, -60.24712676880312046 ) ) ;
#22037 = ORIENTED_EDGE ( 'NONE', *, *, #1802, .F. ) ;
#22038 = CARTESIAN_POINT ( 'NONE',  ( -7.552830808693327569, 40.00000000000000000, -52.78252196372452687 ) ) ;
#22039 = EDGE_CURVE ( 'NONE', #20199, #6208, #636, .T. ) ;
#22040 =( BOUNDED_SURFACE ( )  B_SPLINE_SURFACE ( 3, 2, ( 
 ( #9, #1731, #15695 ),
 ( #7001, #13956, #7874 ),
 ( #4103, #3998, #11073 ),
 ( #16468, #774, #19802 ),
 ( #19907, #14728, #18063 ),
 ( #20027, #4334, #16693 ),
 ( #882, #18405, #21863 ),
 ( #11314, #18300, #7653 ) ),
 .UNSPECIFIED., .F., .F., .F. ) 
 B_SPLINE_SURFACE_WITH_KNOTS ( ( 4, 2, 2, 4 ),
 ( 3, 3 ),
 ( -2.168404344971008868E-18, 0.005619572794283482498, 0.008429359191425223746, 0.01123914558856696673 ),
 ( 0.000000000000000000, 1.000000000000000000 ),
 .UNSPECIFIED. ) 
 GEOMETRIC_REPRESENTATION_ITEM ( )  RATIONAL_B_SPLINE_SURFACE ( (
 ( 1.000000000000000000, 0.7200096751079135826, 1.000000000000000000),
 ( 1.000000000000000000, 0.7496815117904079839, 1.000000000000000000),
 ( 1.000000000000000000, 0.7737746244339125390, 1.000000000000000000),
 ( 1.000000000000000000, 0.8024243379864889336, 1.000000000000000000),
 ( 1.000000000000000000, 0.8107154503870998008, 1.000000000000000000),
 ( 1.000000000000000000, 0.8248921579234514967, 1.000000000000000000),
 ( 1.000000000000000000, 0.8307774003434091892, 1.000000000000000000),
 ( 1.000000000000000000, 0.8354972176269009898, 1.000000000000000000) ) ) 
 REPRESENTATION_ITEM ( '' )  SURFACE ( )  );
#22041 = CARTESIAN_POINT ( 'NONE',  ( 4.589505318347391949, 39.46976832855466455, -53.62193830992116261 ) ) ;
#22042 = ORIENTED_EDGE ( 'NONE', *, *, #16066, .F. ) ;
#22043 = CARTESIAN_POINT ( 'NONE',  ( 42.50000000000000711, -12.00000000000012434, -50.02500000000011227 ) ) ;
#22044 = CARTESIAN_POINT ( 'NONE',  ( -2.995584608082017652, -1.237002266245721405, 50.27666343020542428 ) ) ;
#22045 = ORIENTED_EDGE ( 'NONE', *, *, #20210, .F. ) ;
#22046 = UNCERTAINTY_MEASURE_WITH_UNIT (LENGTH_MEASURE( 1.000000000000000082E-05 ), #17664, 'distance_accuracy_value', 'NONE');
#22047 = CARTESIAN_POINT ( 'NONE',  ( 8.331955809010597847, 38.18181818181818699, 56.36098470834072316 ) ) ;
#22048 = CARTESIAN_POINT ( 'NONE',  ( 34.99999999999999289, -5.000000000000000000, -54.99999999999705835 ) ) ;
#22049 = EDGE_CURVE ( 'NONE', #19899, #14723, #17121, .T. ) ;
#22050 = CARTESIAN_POINT ( 'NONE',  ( 19.96824854984769004, 18.58379861519964393, -58.13906733436663643 ) ) ;
#22051 = ORIENTED_EDGE ( 'NONE', *, *, #19922, .F. ) ;
#22052 = APPLICATION_CONTEXT ( 'automotive_design' ) ;
#22053 = CIRCLE ( 'NONE', #16166, 1.000000000000000888 ) ;
#22054 = ORIENTED_EDGE ( 'NONE', *, *, #20243, .T. ) ;
#22055 = EDGE_LOOP ( 'NONE', ( #14193, #11225 ) ) ;
#22056 = VERTEX_POINT ( 'NONE', #6957 ) ;
#22057 = CARTESIAN_POINT ( 'NONE',  ( 10.80340688045851216, 39.17018323811936398, 54.94414022070431258 ) ) ;
#22058 = DIRECTION ( 'NONE',  ( -1.000000000000000000, 0.000000000000000000, 0.000000000000000000 ) ) ;
#22059 = ORIENTED_EDGE ( 'NONE', *, *, #16328, .F. ) ;
#22060 = DIRECTION ( 'NONE',  ( -1.000000000000000000, 1.775147869274631246E-14, 0.000000000000000000 ) ) ;
#22061 = CARTESIAN_POINT ( 'NONE',  ( -34.99999999999980815, 26.00000000000000355, 54.99999999999922551 ) ) ;
#22062 = EDGE_LOOP ( 'NONE', ( #13271, #19510 ) ) ;
#22063 = CARTESIAN_POINT ( 'NONE',  ( -34.99999999999999289, -5.000000000000000000, 58.99999999999698019 ) ) ;
#22064 = DIRECTION ( 'NONE',  ( 0.000000000000000000, 0.000000000000000000, -1.000000000000000000 ) ) ;
#22065 = ADVANCED_FACE ( 'NONE', ( #3639 ), #5799, .T. ) ;
#22066 = EDGE_LOOP ( 'NONE', ( #10563, #17387, #15646, #10812, #18337, #6757, #396, #7973, #7050, #489, #6960, #17329, #19468, #3290, #7016, #17590, #17417, #15179, #9875, #5086, #2925, #1577, #19060, #16282, #13486, #1189, #13093, #21514, #1477, #18835, #16897, #13960, #19950, #10733, #8211, #21662, #16832, #15036, #4441, #6778, #2164, #8954, #148, #17784, #21349, #80, #3172, #5001, #7586, #4417, #5081, #7852, #10121, #5548, #1172, #17218, #17817, #1944, #11254, #11358, #5363, #7697, #8590, #15273, #12973, #5382, #14489, #18397, #21322, #13441, #13931, #21313, #16852, #13295, #2589, #8148, #17971, #18694, #14835, #12406, #8161, #4600, #19515, #6230, #2510, #4194, #20664, #20785, #1156, #21509, #20900, #19849, #19852, #11144, #10658, #13236, #11590, #20457, #2256, #4902, #758, #7824, #13977, #4165, #1721, #8206, #1462, #13109, #18936, #3123, #9530, #18312, #14549, #7022, #8433, #3344, #3629, #20906, #11823, #19495, #17926, #7154, #2446, #19630, #18378, #20878, #21797, #16135, #2986, #18141, #17931 ) ) ;
#22067 = LINE ( 'NONE', #21614, #7158 ) ;
#22068 = CYLINDRICAL_SURFACE ( 'NONE', #14182, 36.76383501243555685 ) ;
#22069 = B_SPLINE_CURVE_WITH_KNOTS ( 'NONE', 3,
 ( #9552, #11719, #21820, #6118, #13081, #1290, #2917, #11497, #20100, #8284 ),
 .UNSPECIFIED., .F., .F.,
 ( 4, 2, 2, 2, 4 ),
 ( -8.975271422312889897E-06, 0.0006698366896151128867, 0.001348648650652538826, 0.002027460611689964332, 0.002706272572727390271 ),
 .UNSPECIFIED. ) ;
#22070 = CARTESIAN_POINT ( 'NONE',  ( 2.775557561562891351E-14, -2.775557561562891351E-14, 2.999999999999999112 ) ) ;
#22071 = AXIS2_PLACEMENT_3D ( 'NONE', #2531, #9403, #1029 ) ;
#22072 = AXIS2_PLACEMENT_3D ( 'NONE', #17333, #12179, #7024 ) ;
#22073 = EDGE_CURVE ( 'NONE', #16550, #18180, #7243, .T. ) ;
#22074 = EDGE_CURVE ( 'NONE', #15024, #8759, #14017, .T. ) ;
#22075 = AXIS2_PLACEMENT_3D ( 'NONE', #7275, #390, #7386 ) ;
#22076 = CARTESIAN_POINT ( 'NONE',  ( -7.980461308159936706, 36.39375341857520141, -2.999999999999999112 ) ) ;
#22077 = VERTEX_POINT ( 'NONE', #5231 ) ;
#22078 = ORIENTED_EDGE ( 'NONE', *, *, #9735, .T. ) ;
#22079 = EDGE_CURVE ( 'NONE', #17839, #790, #6840, .T. ) ;
#22080 = EDGE_LOOP ( 'NONE', ( #17773, #6899 ) ) ;
#22081 = CARTESIAN_POINT ( 'NONE',  ( -19.27753112432710481, 25.39788459339701987, 57.95296232962699179 ) ) ;
#22082 = FACE_OUTER_BOUND ( 'NONE', #10891, .T. ) ;
#22083 = B_SPLINE_SURFACE_WITH_KNOTS ( 'NONE', 3, 1, ( 
 ( #12257, #5728 ),
 ( #1945, #1843 ),
 ( #19723, #14300 ),
 ( #10635, #14185 ),
 ( #19595, #2060 ),
 ( #8933, #19263 ),
 ( #106, #21423 ),
 ( #4028, #3683 ),
 ( #10870, #15906 ),
 ( #17875, #9162 ) ),
 .UNSPECIFIED., .F., .F., .F.,
 ( 4, 2, 2, 2, 4 ),
 ( 2, 2 ),
 ( 0.000000000000000000, 0.2500000000000000000, 0.5000000000000000000, 0.7500000000000000000, 1.000000000000000000 ),
 ( 0.000000000000000000, 1.000000000000000000 ),
 .UNSPECIFIED. ) ;
#22084 = CIRCLE ( 'NONE', #15096, 15.00000000000000000 ) ;
#22085 = VECTOR ( 'NONE', #6000, 1000.000000000000000 ) ;
#22086 = CARTESIAN_POINT ( 'NONE',  ( 42.50000000000000711, -9.600000000000001421, -47.50000000000000000 ) ) ;
#22087 = CARTESIAN_POINT ( 'NONE',  ( 2.775557561562891351E-14, 2.775557561562891351E-14, 5.750000000000001776 ) ) ;
#22088 = CIRCLE ( 'NONE', #12916, 1.000000000000000888 ) ;
#22089 = DIRECTION ( 'NONE',  ( -0.000000000000000000, 1.000000000000000000, -0.000000000000000000 ) ) ;
#22090 = ORIENTED_EDGE ( 'NONE', *, *, #12206, .T. ) ;
#22091 = CARTESIAN_POINT ( 'NONE',  ( -34.99999999999999289, -3.999999999999985345, -3.012171160963566127E-14 ) ) ;
#22092 = CARTESIAN_POINT ( 'NONE',  ( -4.997499695308150081E-15, -0.2027466127521987682, 49.39731220485085572 ) ) ;
#22093 = CARTESIAN_POINT ( 'NONE',  ( -42.49999999999996447, 10.00000000000000000, -47.50000000000000711 ) ) ;
#22094 = CARTESIAN_POINT ( 'NONE',  ( -8.331955809010668901, 38.18181818181816567, -56.36098470834073737 ) ) ;
#22095 = FACE_OUTER_BOUND ( 'NONE', #7048, .T. ) ;
#22096 = VERTEX_POINT ( 'NONE', #5879 ) ;
#22097 = CARTESIAN_POINT ( 'NONE',  ( -24.73600648735116536, 27.19760187735834123, -1.999999999999977573 ) ) ;
#22098 = LINE ( 'NONE', #8225, #7868 ) ;
#22099 = ORIENTED_EDGE ( 'NONE', *, *, #8746, .F. ) ;
#22100 = B_SPLINE_CURVE_WITH_KNOTS ( 'NONE', 3,
 ( #8340, #10044, #11769, #6737, #13242, #16712, #2742, #8454, #2857, #15314 ),
 .UNSPECIFIED., .F., .F.,
 ( 4, 2, 2, 2, 4 ),
 ( 0.000000000000000000, 0.002975785561748156127, 0.005951571123496312253, 0.008927356685244467946, 0.01190314224699262451 ),
 .UNSPECIFIED. ) ;
#22101 = AXIS2_PLACEMENT_3D ( 'NONE', #13984, #10230, #14100 ) ;
#22102 = DIRECTION ( 'NONE',  ( 0.000000000000000000, 0.000000000000000000, 1.000000000000000000 ) ) ;
#22103 = DIRECTION ( 'NONE',  ( 6.505213034913038160E-19, 3.903127820947822896E-18, 1.000000000000000000 ) ) ;
#22104 = DIRECTION ( 'NONE',  ( -1.000000000000000000, -1.208970125616063644E-17, 0.000000000000000000 ) ) ;
#22105 = AXIS2_PLACEMENT_3D ( 'NONE', #3775, #10981, #19814 ) ;
#22106 = CIRCLE ( 'NONE', #12554, 31.50000000000001421 ) ;
#22107 = EDGE_CURVE ( 'NONE', #3556, #5472, #1386, .T. ) ;
#22108 = EDGE_LOOP ( 'NONE', ( #12941, #6431 ) ) ;
#22109 = EDGE_CURVE ( 'NONE', #4439, #15664, #14253, .T. ) ;
#22110 = VERTEX_POINT ( 'NONE', #19441 ) ;
#22111 = CARTESIAN_POINT ( 'NONE',  ( -42.50000000000000711, -12.00000000000012434, 44.97499999999989484 ) ) ;
#22112 = ADVANCED_FACE ( 'NONE', ( #21041 ), #7054, .T. ) ;
#22113 = DIRECTION ( 'NONE',  ( 6.505213034913038160E-19, 3.903127820947822896E-18, 1.000000000000000000 ) ) ;
#22114 = VERTEX_POINT ( 'NONE', #12101 ) ;
#22115 = DIRECTION ( 'NONE',  ( -1.000000000000000000, -1.208970125616063644E-17, 0.000000000000000000 ) ) ;
#22116 = DIRECTION ( 'NONE',  ( 6.505213034913038160E-19, 3.903127820947822896E-18, 1.000000000000000000 ) ) ;
#22117 = CARTESIAN_POINT ( 'NONE',  ( -9.689843208404459673, 39.33333333333334991, -54.54983754392748807 ) ) ;
#22118 = AXIS2_PLACEMENT_3D ( 'NONE', #2877, #2762, #22240 ) ;
#22119 = LINE ( 'NONE', #18443, #5677 ) ;
#22120 = DIRECTION ( 'NONE',  ( -6.505213034913038160E-19, -3.903127820947822896E-18, -1.000000000000000000 ) ) ;
#22121 = ORIENTED_EDGE ( 'NONE', *, *, #2948, .T. ) ;
#22122 = DIRECTION ( 'NONE',  ( 1.000000000000000000, 0.000000000000000000, 0.000000000000000000 ) ) ;
#22123 = CARTESIAN_POINT ( 'NONE',  ( 35.00000000000000000, 7.000000000000000000, 2.365113165210053967E-14 ) ) ;
#22124 = DIRECTION ( 'NONE',  ( -1.000000000000000000, 1.204669080539449590E-16, 0.000000000000000000 ) ) ;
#22125 = FACE_OUTER_BOUND ( 'NONE', #473, .T. ) ;
#22126 = ORIENTED_EDGE ( 'NONE', *, *, #2163, .F. ) ;
#22127 = AXIS2_PLACEMENT_3D ( 'NONE', #16978, #11492, #20436 ) ;
#22128 = CARTESIAN_POINT ( 'NONE',  ( -28.50000000000001421, 19.99999999999982947, -105.0000000000000142 ) ) ;
#22129 = CARTESIAN_POINT ( 'NONE',  ( -10.50000000000012079, 42.51666049839536043, -105.0000000000000142 ) ) ;
#22130 = CIRCLE ( 'NONE', #15150, 2.500000000000002220 ) ;
#22131 = PRODUCT_DEFINITION_SHAPE ( 'NONE', 'NONE',  #22697 ) ;
#22132 = CONICAL_SURFACE ( 'NONE', #19209, 39.00000000000001421, 0.7853981633974447263 ) ;
#22133 = EDGE_LOOP ( 'NONE', ( #5059, #19071, #7470, #8223 ) ) ;
#22134 = VERTEX_POINT ( 'NONE', #1681 ) ;
#22135 = SHAPE_DEFINITION_REPRESENTATION ( #4005, #6502 ) ;
#22136 = ORIENTED_EDGE ( 'NONE', *, *, #7114, .T. ) ;
#22137 = CARTESIAN_POINT ( 'NONE',  ( 9.940687323067940895, 37.37897894777886876, 57.14641600008368982 ) ) ;
#22138 = LINE ( 'NONE', #6436, #16511 ) ;
#22139 = CARTESIAN_POINT ( 'NONE',  ( -34.99999999999998579, 0.000000000000000000, 58.99999999999697309 ) ) ;
#22140 = CYLINDRICAL_SURFACE ( 'NONE', #6504, 2.499999999999995115 ) ;
#22141 = CIRCLE ( 'NONE', #13330, 19.11328065563152379 ) ;
#22142 = DIRECTION ( 'NONE',  ( -1.000000000000000000, -1.208970125616060101E-17, 6.505213034913038160E-19 ) ) ;
#22143 = ORIENTED_EDGE ( 'NONE', *, *, #17587, .F. ) ;
#22144 = CARTESIAN_POINT ( 'NONE',  ( -35.00000000000000000, 17.00000000000000000, 17.00000000000002487 ) ) ;
#22145 = CARTESIAN_POINT ( 'NONE',  ( 31.41173278719269746, 17.66631876130919565, 2.999999999999999112 ) ) ;
#22146 = ORIENTED_EDGE ( 'NONE', *, *, #6306, .F. ) ;
#22147 = CARTESIAN_POINT ( 'NONE',  ( 3.877306978638209416E-14, -1.500000000000015099, -12.00000000000000355 ) ) ;
#22148 = EDGE_CURVE ( 'NONE', #2722, #20782, #6892, .T. ) ;
#22149 = LINE ( 'NONE', #22266, #10830 ) ;
#22150 = CARTESIAN_POINT ( 'NONE',  ( -10.00000000000000888, 2.999999999999836131, -4.999999999999948486 ) ) ;
#22151 = CARTESIAN_POINT ( 'NONE',  ( 4.025500340002596822, -36.54278193890326065, -2.000000000000005329 ) ) ;
#22152 = VERTEX_POINT ( 'NONE', #12212 ) ;
#22153 = DIRECTION ( 'NONE',  ( -0.000000000000000000, 1.000000000000000000, -0.000000000000000000 ) ) ;
#22154 = EDGE_LOOP ( 'NONE', ( #6851, #20784, #19350, #8046 ) ) ;
#22155 = CARTESIAN_POINT ( 'NONE',  ( 7.505578006075174891, 1.461761173328240071, -55.63523492904086254 ) ) ;
#22156 = VERTEX_POINT ( 'NONE', #3520 ) ;
#22157 = CARTESIAN_POINT ( 'NONE',  ( -24.75236754129142724, -27.84804035626034491, -6.999999999999999112 ) ) ;
#22158 = EDGE_CURVE ( 'NONE', #3688, #5859, #21580, .T. ) ;
#22159 = PLANE ( 'NONE',  #6053 ) ;
#22160 = DIRECTION ( 'NONE',  ( 1.000000000000000000, 0.000000000000000000, 0.000000000000000000 ) ) ;
#22161 = AXIS2_PLACEMENT_3D ( 'NONE', #12195, #8011, #14966 ) ;
#22162 = VECTOR ( 'NONE', #16499, 1000.000000000000000 ) ;
#22163 = CARTESIAN_POINT ( 'NONE',  ( 19.23518390577179105, 25.54875756131788123, -60.43569366689261813 ) ) ;
#22164 = ORIENTED_EDGE ( 'NONE', *, *, #7070, .F. ) ;
#22165 = AXIS2_PLACEMENT_3D ( 'NONE', #14514, #19390, #1959 ) ;
#22166 = ORIENTED_EDGE ( 'NONE', *, *, #4221, .T. ) ;
#22167 = EDGE_LOOP ( 'NONE', ( #9424, #4887, #20909, #16179 ) ) ;
#22168 = ORIENTED_EDGE ( 'NONE', *, *, #13850, .F. ) ;
#22169 = CARTESIAN_POINT ( 'NONE',  ( 0.3961047786450465069, 24.97928910538451319, 6.993377406885177727 ) ) ;
#22170 =( BOUNDED_SURFACE ( )  B_SPLINE_SURFACE ( 3, 2, ( 
 ( #13063, #16964, #3003 ),
 ( #8265, #11247, #18245 ),
 ( #2556, #11362, #9535 ),
 ( #821, #7811, #14786 ),
 ( #21803, #19039, #8718 ),
 ( #19148, #18921, #10197 ),
 ( #6658, #19265, #1389 ),
 ( #3568, #8825, #15796 ),
 ( #17190, #15351, #3346 ),
 ( #1502, #5285, #22599 ) ),
 .UNSPECIFIED., .F., .F., .F. ) 
 B_SPLINE_SURFACE_WITH_KNOTS ( ( 4, 2, 2, 2, 4 ),
 ( 3, 3 ),
 ( 0.02809317535148810746, 0.03071213539477267440, 0.03333109543805724134, 0.03595005548134180828, 0.03856901552462637522 ),
 ( 0.2389732943673020804, 1.000000000000000000 ),
 .UNSPECIFIED. ) 
 GEOMETRIC_REPRESENTATION_ITEM ( )  RATIONAL_B_SPLINE_SURFACE ( (
 ( 0.9723126933862670240, 0.9420702913958711733, 1.000000000000000000),
 ( 0.9749922925144016705, 0.9476767737754799859, 1.000000000000000000),
 ( 0.9774153414777251303, 0.9527464803503058466, 1.000000000000000000),
 ( 0.9815341666525440045, 0.9613642323583782012, 1.000000000000000000),
 ( 0.9832251939808056562, 0.9649023417792208512, 1.000000000000000000),
 ( 0.9856873122312799218, 0.9700537923984060562, 1.000000000000000000),
 ( 0.9864553338148209782, 0.9716607116685581635, 1.000000000000000000),
 ( 0.9870557760262803626, 0.9729170072999364649, 1.000000000000000000),
 ( 0.9868934176577699446, 0.9725773074833932164, 1.000000000000000000),
 ( 0.9863383242652692395, 0.9714158944602974133, 1.000000000000000000) ) ) 
 REPRESENTATION_ITEM ( '' )  SURFACE ( )  );
#22171 = ORIENTED_EDGE ( 'NONE', *, *, #2427, .T. ) ;
#22172 = CARTESIAN_POINT ( 'NONE',  ( -5.074925817841801745, 32.10132595304121850, -6.999999999999950262 ) ) ;
#22173 = LINE ( 'NONE', #9798, #21625 ) ;
#22174 = EDGE_LOOP ( 'NONE', ( #22340, #21650, #13369, #21761, #11339 ) ) ;
#22175 = CIRCLE ( 'NONE', #13715, 2.999999999999999112 ) ;
#22176 = EDGE_CURVE ( 'NONE', #2120, #20382, #5457, .T. ) ;
#22177 = DIRECTION ( 'NONE',  ( 0.000000000000000000, -1.000000000000000000, 0.000000000000000000 ) ) ;
#22178 = AXIS2_PLACEMENT_3D ( 'NONE', #14022, #1806, #15760 ) ;
#22179 = AXIS2_PLACEMENT_3D ( 'NONE', #985, #5914, #9355 ) ;
#22180 = CARTESIAN_POINT ( 'NONE',  ( 25.00000000000000000, -20.00000000000000000, 6.487780019669002523E-15 ) ) ;
#22181 = ORIENTED_EDGE ( 'NONE', *, *, #19252, .T. ) ;
#22182 = DIRECTION ( 'NONE',  ( 0.000000000000000000, 0.000000000000000000, 1.000000000000000000 ) ) ;
#22183 = AXIS2_PLACEMENT_3D ( 'NONE', #14291, #15685, #21192 ) ;
#22184 = FACE_OUTER_BOUND ( 'NONE', #21356, .T. ) ;
#22185 = DIRECTION ( 'NONE',  ( -1.000000000000000000, 1.243413522203471269E-14, 0.000000000000000000 ) ) ;
#22186 = CARTESIAN_POINT ( 'NONE',  ( -0.2661007013785012809, 39.99958209025860612, 48.93999295480112721 ) ) ;
#22187 = VECTOR ( 'NONE', #11544, 1000.000000000000000 ) ;
#22188 = CARTESIAN_POINT ( 'NONE',  ( -15.00000000000001421, 20.00000000000000355, 45.82575694955841072 ) ) ;
#22189 = AXIS2_PLACEMENT_3D ( 'NONE', #21401, #319, #2037 ) ;
#22190 = AXIS2_PLACEMENT_3D ( 'NONE', #19219, #15864, #9438 ) ;
#22191 = CIRCLE ( 'NONE', #19260, 34.90673715956759082 ) ;
#22192 = ORIENTED_EDGE ( 'NONE', *, *, #13017, .F. ) ;
#22193 = CIRCLE ( 'NONE', #592, 2.499999999999995115 ) ;
#22194 = VERTEX_POINT ( 'NONE', #10482 ) ;
#22195 = EDGE_CURVE ( 'NONE', #20081, #1054, #7630, .T. ) ;
#22196 = VERTEX_POINT ( 'NONE', #17481 ) ;
#22197 = CARTESIAN_POINT ( 'NONE',  ( -17.57556337525805290, 10.44046169743836217, 57.45538260706025824 ) ) ;
#22198 = CIRCLE ( 'NONE', #18888, 6.499999999999999112 ) ;
#22199 = DIRECTION ( 'NONE',  ( -1.000000000000000000, 0.000000000000000000, 0.000000000000000000 ) ) ;
#22200 = CARTESIAN_POINT ( 'NONE',  ( -19.80807096600700845, 16.80592363802972145, -60.57763526510198915 ) ) ;
#22201 = CARTESIAN_POINT ( 'NONE',  ( 7.031141211283101100, 39.67715641065061760, 53.36152252427557130 ) ) ;
#22202 = EDGE_CURVE ( 'NONE', #10068, #18961, #8883, .T. ) ;
#22203 = EDGE_CURVE ( 'NONE', #12412, #10093, #294, .T. ) ;
#22204 = FACE_OUTER_BOUND ( 'NONE', #12147, .T. ) ;
#22205 = ORIENTED_EDGE ( 'NONE', *, *, #5943, .F. ) ;
#22206 = DIRECTION ( 'NONE',  ( -1.000000000000000000, -1.208970125616044077E-17, 0.000000000000000000 ) ) ;
#22207 = CARTESIAN_POINT ( 'NONE',  ( -35.00000000000000000, 0.000000000000000000, 1.387778780781445676E-14 ) ) ;
#22208 = DIRECTION ( 'NONE',  ( 1.000000000000000000, 0.000000000000000000, 0.000000000000000000 ) ) ;
#22209 = AXIS2_PLACEMENT_3D ( 'NONE', #18226, #11226, #16616 ) ;
#22210 = VERTEX_POINT ( 'NONE', #14134 ) ;
#22211 = EDGE_CURVE ( 'NONE', #22660, #13179, #3744, .T. ) ;
#22212 = CARTESIAN_POINT ( 'NONE',  ( -11.86180952234344588, 38.99999999999292299, 55.35904751185378103 ) ) ;
#22213 = CARTESIAN_POINT ( 'NONE',  ( 14.70622169671638169, 6.333487747693914649, 56.50111465620437912 ) ) ;
#22214 = VECTOR ( 'NONE', #766, 1000.000000000000000 ) ;
#22215 = ORIENTED_EDGE ( 'NONE', *, *, #14202, .T. ) ;
#22216 = LINE ( 'NONE', #8452, #3609 ) ;
#22217 = DIRECTION ( 'NONE',  ( -0.7752116086454780008, 0.5577761202038526989, -0.2965345874457614439 ) ) ;
#22218 = CARTESIAN_POINT ( 'NONE',  ( 7.310544252644470693E-15, 28.19616000222403684, 0.000000000000000000 ) ) ;
#22219 = CARTESIAN_POINT ( 'NONE',  ( 6.696867368502865039E-15, 35.00000000000000000, 38.73397172404480671 ) ) ;
#22220 = EDGE_CURVE ( 'NONE', #4376, #15814, #1452, .T. ) ;
#22221 = EDGE_LOOP ( 'NONE', ( #5188, #1868, #16992, #9002 ) ) ;
#22222 = ADVANCED_FACE ( 'NONE', ( #17705 ), #15012, .F. ) ;
#22223 = CIRCLE ( 'NONE', #22239, 19.11328065563151668 ) ;
#22224 = AXIS2_PLACEMENT_3D ( 'NONE', #11082, #5587, #11199 ) ;
#22225 = VERTEX_POINT ( 'NONE', #7815 ) ;
#22226 = CARTESIAN_POINT ( 'NONE',  ( -6.674721970908912283, -4.820493483656560052, 49.68071724292274638 ) ) ;
#22227 = CARTESIAN_POINT ( 'NONE',  ( -1.387778780781445676E-14, 20.00000000000000000, 102.0000000000000142 ) ) ;
#22228 = ORIENTED_EDGE ( 'NONE', *, *, #2140, .T. ) ;
#22229 = LINE ( 'NONE', #15210, #21982 ) ;
#22230 = DIRECTION ( 'NONE',  ( 0.000000000000000000, 1.000000000000000000, 0.000000000000000000 ) ) ;
#22231 = DIRECTION ( 'NONE',  ( -1.000000000000000000, 0.000000000000000000, 0.000000000000000000 ) ) ;
#22232 = CARTESIAN_POINT ( 'NONE',  ( -18.64599517736102996, 12.71385791664993370, -57.77541544179386790 ) ) ;
#22233 = ADVANCED_FACE ( 'NONE', ( #21807 ), #11644, .T. ) ;
#22234 = CARTESIAN_POINT ( 'NONE',  ( -8.553361841769476115, 39.50247004197922251, 54.09836511283659632 ) ) ;
#22235 = CIRCLE ( 'NONE', #10872, 31.50000000000001421 ) ;
#22236 = DIRECTION ( 'NONE',  ( 0.9012767464701764153, 6.280369834735124333E-16, -0.4332438415859287129 ) ) ;
#22237 = VERTEX_POINT ( 'NONE', #9646 ) ;
#22238 = CARTESIAN_POINT ( 'NONE',  ( 13.59841332577230411, 26.34257281673386686, 45.18857684126744090 ) ) ;
#22239 = AXIS2_PLACEMENT_3D ( 'NONE', #8389, #22608, #11930 ) ;
#22240 = DIRECTION ( 'NONE',  ( 1.000000000000000000, 1.208970125616053321E-17, 0.000000000000000000 ) ) ;
#22241 = FACE_OUTER_BOUND ( 'NONE', #16438, .T. ) ;
#22242 = CARTESIAN_POINT ( 'NONE',  ( 35.29097153256788744, 4.153395668489309855, -2.999999999999986677 ) ) ;
#22243 = AXIS2_PLACEMENT_3D ( 'NONE', #7088, #12028, #13842 ) ;
#22244 = ORIENTED_EDGE ( 'NONE', *, *, #20258, .T. ) ;
#22245 = DIRECTION ( 'NONE',  ( -1.000000000000000000, 0.000000000000000000, 0.000000000000000000 ) ) ;
#22246 = CARTESIAN_POINT ( 'NONE',  ( 5.010575289839681368, 5.833430802647523450, 40.02075074423078149 ) ) ;
#22247 = CIRCLE ( 'NONE', #15631, 19.00000000000000355 ) ;
#22248 = CIRCLE ( 'NONE', #3206, 2.500000000000008882 ) ;
#22249 = ORIENTED_EDGE ( 'NONE', *, *, #1598, .T. ) ;
#22250 = CIRCLE ( 'NONE', #5061, 2.099999999999997868 ) ;
#22251 = CIRCLE ( 'NONE', #10140, 19.00000000000000355 ) ;
#22252 = EDGE_LOOP ( 'NONE', ( #14935, #20137, #8406, #3772 ) ) ;
#22253 = AXIS2_PLACEMENT_3D ( 'NONE', #2033, #5700, #10388 ) ;
#22254 = EDGE_LOOP ( 'NONE', ( #2782, #993, #3993, #20653 ) ) ;
#22255 = PLANE ( 'NONE',  #14687 ) ;
#22256 = DIRECTION ( 'NONE',  ( 0.000000000000000000, 0.000000000000000000, -1.000000000000000000 ) ) ;
#22257 = CARTESIAN_POINT ( 'NONE',  ( 35.00000000000000000, 25.00000000000000000, 4.258610482196280173E-15 ) ) ;
#22258 = DIRECTION ( 'NONE',  ( -0.000000000000000000, 1.000000000000000000, -0.000000000000000000 ) ) ;
#22259 = CARTESIAN_POINT ( 'NONE',  ( -12.99999999999980282, -2.516660498395516310, 105.0000000000000142 ) ) ;
#22260 = ORIENTED_EDGE ( 'NONE', *, *, #8351, .F. ) ;
#22261 = FACE_OUTER_BOUND ( 'NONE', #19887, .T. ) ;
#22262 = DIRECTION ( 'NONE',  ( 1.000000000000000000, 0.000000000000000000, 0.000000000000000000 ) ) ;
#22263 = ORIENTED_EDGE ( 'NONE', *, *, #10026, .T. ) ;
#22264 = CARTESIAN_POINT ( 'NONE',  ( -7.017626609043932540, 6.725442770851636887, -41.44244536674932533 ) ) ;
#22265 = EDGE_CURVE ( 'NONE', #15997, #17185, #7937, .T. ) ;
#22266 = CARTESIAN_POINT ( 'NONE',  ( 4.163799117100995136E-16, 30.00000000000000000, -3.399999999999995026 ) ) ;
#22267 = CARTESIAN_POINT ( 'NONE',  ( -14.74639653023206165, 28.96193690644924246, -2.999999999999968026 ) ) ;
#22268 = CARTESIAN_POINT ( 'NONE',  ( -1.387778780781494900E-14, 40.00000000000002132, 48.73397172404481381 ) ) ;
#22269 = EDGE_LOOP ( 'NONE', ( #13309, #3369, #18178 ) ) ;
#22270 = CARTESIAN_POINT ( 'NONE',  ( 35.52192638951989068, -1.010906942018348520, 3.000000000000051514 ) ) ;
#22271 = AXIS2_PLACEMENT_3D ( 'NONE', #18914, #3223, #16543 ) ;
#22272 = VERTEX_POINT ( 'NONE', #18700 ) ;
#22273 = DIRECTION ( 'NONE',  ( 0.000000000000000000, 0.000000000000000000, -1.000000000000000000 ) ) ;
#22274 = CARTESIAN_POINT ( 'NONE',  ( -19.73349596156088381, 30.70641346160536855, 58.02568834892373673 ) ) ;
#22275 = AXIS2_PLACEMENT_3D ( 'NONE', #8301, #7848, #11623 ) ;
#22276 = ORIENTED_EDGE ( 'NONE', *, *, #2366, .T. ) ;
#22277 = DIRECTION ( 'NONE',  ( 0.000000000000000000, 0.000000000000000000, 1.000000000000000000 ) ) ;
#22278 = AXIS2_PLACEMENT_3D ( 'NONE', #4289, #16421, #5996 ) ;
#22279 = EDGE_CURVE ( 'NONE', #14544, #19784, #6158, .T. ) ;
#22280 = VECTOR ( 'NONE', #7060, 1000.000000000000000 ) ;
#22281 = LINE ( 'NONE', #6575, #14460 ) ;
#22282 = CARTESIAN_POINT ( 'NONE',  ( 2.220446049250313081E-13, 2.775557561562891351E-14, -2.800654218530485018 ) ) ;
#22283 = VECTOR ( 'NONE', #17597, 1000.000000000000000 ) ;
#22284 = CARTESIAN_POINT ( 'NONE',  ( 19.98434069128079216, 21.18673122687495436, -60.61816909401677123 ) ) ;
#22286 = ORIENTED_EDGE ( 'NONE', *, *, #13080, .T. ) ;
#22285 = EDGE_CURVE ( 'NONE', #8864, #19508, #15909, .T. ) ;
#22288 = ORIENTED_EDGE ( 'NONE', *, *, #4464, .F. ) ;
#22287 = B_SPLINE_CURVE_WITH_KNOTS ( 'NONE', 3,
 ( #461, #18334, #11349, #2650 ),
 .UNSPECIFIED., .F., .F.,
 ( 4, 4 ),
 ( 9.545285769853128040E-07, 0.001900595205834734389 ),
 .UNSPECIFIED. ) ;
#22289 = AXIS2_PLACEMENT_3D ( 'NONE', #2244, #14490, #3857 ) ;
#22290 = ORIENTED_EDGE ( 'NONE', *, *, #3104, .T. ) ;
#22291 = AXIS2_PLACEMENT_3D ( 'NONE', #19043, #13862, #18927 ) ;
#22292 =( NAMED_UNIT ( * ) SI_UNIT ( $, .STERADIAN. ) SOLID_ANGLE_UNIT ( ) );
#22293 = ORIENTED_EDGE ( 'NONE', *, *, #8400, .F. ) ;
#22294 = DIRECTION ( 'NONE',  ( 0.000000000000000000, -1.000000000000000000, 0.000000000000000000 ) ) ;
#22295 = CIRCLE ( 'NONE', #11658, 17.00000000000000000 ) ;
#22296 = LINE ( 'NONE', #11513, #1230 ) ;
#22297 = ADVANCED_FACE ( 'NONE', ( #12959 ), #2516, .F. ) ;
#22298 = CARTESIAN_POINT ( 'NONE',  ( -34.99999999999999289, 40.00000000000000000, 50.00000000000000000 ) ) ;
#22299 = ORIENTED_EDGE ( 'NONE', *, *, #3851, .T. ) ;
#22300 = CARTESIAN_POINT ( 'NONE',  ( 0.000000000000000000, -1.500000000000015099, 0.000000000000000000 ) ) ;
#22301 = CARTESIAN_POINT ( 'NONE',  ( 1.511556752574976237, 13.38245151354841056, 6.879730668893286882 ) ) ;
#22302 = ORIENTED_EDGE ( 'NONE', *, *, #20251, .T. ) ;
#22303 = AXIS2_PLACEMENT_3D ( 'NONE', #1392, #22602, #10307 ) ;
#22304 = DIRECTION ( 'NONE',  ( 6.505213034913038160E-19, 3.903127820947822896E-18, 1.000000000000000000 ) ) ;
#22305 = ORIENTED_EDGE ( 'NONE', *, *, #20625, .F. ) ;
#22306 = FACE_BOUND ( 'NONE', #5757, .T. ) ;
#22307 = DIRECTION ( 'NONE',  ( -0.000000000000000000, -0.000000000000000000, -1.000000000000000000 ) ) ;
#22308 = CARTESIAN_POINT ( 'NONE',  ( -2.836563456948004695E-15, -1.236374842841498678, -48.24164917503444627 ) ) ;
#22309 = CARTESIAN_POINT ( 'NONE',  ( -0.2763205028094647964, 39.99954928602512894, 48.94785969531869085 ) ) ;
#22310 = AXIS2_PLACEMENT_3D ( 'NONE', #16455, #762, #16102 ) ;
#22311 = AXIS2_PLACEMENT_3D ( 'NONE', #3008, #13283, #20197 ) ;
#22312 = CARTESIAN_POINT ( 'NONE',  ( -5.833333333333327708, 6.180730040185831164, 40.61164310337068173 ) ) ;
#22313 =( GEOMETRIC_REPRESENTATION_CONTEXT ( 3 ) GLOBAL_UNCERTAINTY_ASSIGNED_CONTEXT ( ( #14917 ) ) GLOBAL_UNIT_ASSIGNED_CONTEXT ( ( #4491, #18459, #15004 ) ) REPRESENTATION_CONTEXT ( 'NONE', 'WORKASPACE' ) );
#22315 = ORIENTED_EDGE ( 'NONE', *, *, #17587, .T. ) ;
#22314 = ADVANCED_FACE ( 'NONE', ( #6322 ), #20086, .F. ) ;
#22316 = EDGE_LOOP ( 'NONE', ( #9368, #16080, #14928, #7938 ) ) ;
#22317 =( BOUNDED_SURFACE ( )  B_SPLINE_SURFACE ( 3, 2, ( 
 ( #2862, #12015, #17047 ),
 ( #13249, #15203, #9846 ),
 ( #13587, #16834, #22449 ),
 ( #6742, #13708, #20724 ),
 ( #4913, #15087, #1135 ),
 ( #10165, #20498, #11889 ),
 ( #4804, #8348, #22226 ),
 ( #8127, #15321, #18776 ),
 ( #1474, #5033, #20391 ),
 ( #22342, #11773, #6405 ) ),
 .UNSPECIFIED., .F., .F., .F. ) 
 B_SPLINE_SURFACE_WITH_KNOTS ( ( 4, 2, 2, 2, 4 ),
 ( 3, 3 ),
 ( 0.02858426235558113315, 0.03123866089385130690, 0.03389305943212148065, 0.03654745797039165439, 0.03920185650866182814 ),
 ( 0.2389733096698791748, 1.000000000000000000 ),
 .UNSPECIFIED. ) 
 GEOMETRIC_REPRESENTATION_ITEM ( )  RATIONAL_B_SPLINE_SURFACE ( (
 ( 0.9863379792457529494, 0.9714151744119040588, 1.000000000000000000),
 ( 0.9868982363996166018, 0.9725873914152123323, 1.000000000000000000),
 ( 0.9870568516195763475, 0.9729192594806854721, 1.000000000000000000),
 ( 0.9864435726088423007, 0.9716361057017525171, 1.000000000000000000),
 ( 0.9856669209476500715, 0.9700111299622751204, 1.000000000000000000),
 ( 0.9831963891542060408, 0.9648420761527581879, 1.000000000000000000),
 ( 0.9815057839369669690, 0.9613048501345585750, 1.000000000000000000),
 ( 0.9773970105179623502, 0.9527081298048269975, 1.000000000000000000),
 ( 0.9749831541131945833, 0.9476576569965825536, 1.000000000000000000),
 ( 0.9723126921700375735, 0.9420702925606835310, 1.000000000000000000) ) ) 
 REPRESENTATION_ITEM ( '' )  SURFACE ( )  );
#22318 = ORIENTED_EDGE ( 'NONE', *, *, #13136, .T. ) ;
#22319 = ORIENTED_EDGE ( 'NONE', *, *, #17917, .T. ) ;
#22320 = CARTESIAN_POINT ( 'NONE',  ( -21.32594275109384085, 27.02633437841200603, 58.42208514511725781 ) ) ;
#22321 = EDGE_CURVE ( 'NONE', #15970, #11834, #12010, .T. ) ;
#22322 = FACE_OUTER_BOUND ( 'NONE', #20048, .T. ) ;
#22323 = DIRECTION ( 'NONE',  ( -1.000000000000000000, -1.208970125616044077E-17, 0.000000000000000000 ) ) ;
#22324 = DIRECTION ( 'NONE',  ( -0.000000000000000000, -0.000000000000000000, 1.000000000000000000 ) ) ;
#22325 = LINE ( 'NONE', #6609, #7540 ) ;
#22326 = VERTEX_POINT ( 'NONE', #4616 ) ;
#22327 = LINE ( 'NONE', #6611, #15666 ) ;
#22328 = CARTESIAN_POINT ( 'NONE',  ( -7.313763316233817591, 40.00000000000000000, -52.68151668814096666 ) ) ;
#22329 = DIRECTION ( 'NONE',  ( -0.000000000000000000, -0.000000000000000000, -1.000000000000000000 ) ) ;
#22330 = DIRECTION ( 'NONE',  ( 6.505213034913038160E-19, 3.903127820947822896E-18, 1.000000000000000000 ) ) ;
#22331 = EDGE_CURVE ( 'NONE', #16050, #19216, #13178, .T. ) ;
#22332 = ORIENTED_EDGE ( 'NONE', *, *, #2612, .F. ) ;
#22333 = CARTESIAN_POINT ( 'NONE',  ( 42.50000000000000711, -5.000000000000000000, -41.00000000000000000 ) ) ;
#22334 = VERTEX_POINT ( 'NONE', #724 ) ;
#22335 = DIRECTION ( 'NONE',  ( -0.000000000000000000, -1.000000000000000000, -0.000000000000000000 ) ) ;
#22336 = AXIS2_PLACEMENT_3D ( 'NONE', #6616, #13578, #20593 ) ;
#22337 = DIRECTION ( 'NONE',  ( 0.000000000000000000, -1.000000000000000000, 0.000000000000000000 ) ) ;
#22338 = CARTESIAN_POINT ( 'NONE',  ( -5.833333333333328596, 33.81926995981417861, 40.61164310337068173 ) ) ;
#22339 = EDGE_CURVE ( 'NONE', #18643, #20516, #7706, .T. ) ;
#22340 = ORIENTED_EDGE ( 'NONE', *, *, #17594, .F. ) ;
#22341 = ORIENTED_EDGE ( 'NONE', *, *, #8745, .T. ) ;
#22342 = CARTESIAN_POINT ( 'NONE',  ( -9.079900094432140634, 0.2952490899071177899, 53.92155887445841955 ) ) ;
#22343 = DIRECTION ( 'NONE',  ( -1.000000000000000000, -1.208970125616063644E-17, 0.000000000000000000 ) ) ;
#22344 = VERTEX_POINT ( 'NONE', #14680 ) ;
#22345 = FACE_OUTER_BOUND ( 'NONE', #16238, .T. ) ;
#22346 = DIRECTION ( 'NONE',  ( 1.000000000000000000, 0.000000000000000000, 0.000000000000000000 ) ) ;
#22347 = CARTESIAN_POINT ( 'NONE',  ( 10.34893680499437707, -34.64233806479136035, 2.932969818539088003 ) ) ;
#22348 = CARTESIAN_POINT ( 'NONE',  ( -19.39432138270236550, 15.03492235294285884, -60.47577240662248954 ) ) ;
#22349 = CARTESIAN_POINT ( 'NONE',  ( -4.080045426412826082, 32.20238537491812281, -6.999999999999999112 ) ) ;
#22350 = CARTESIAN_POINT ( 'NONE',  ( -13.71171267331838273, 34.59605702017515938, 56.12298047978917026 ) ) ;
#22351 = ADVANCED_FACE ( 'NONE', ( #20195 ), #3621, .F. ) ;
#22352 = ORIENTED_EDGE ( 'NONE', *, *, #12378, .T. ) ;
#22353 = DIRECTION ( 'NONE',  ( -0.000000000000000000, -1.000000000000000000, -0.000000000000000000 ) ) ;
#22354 = DIRECTION ( 'NONE',  ( 0.000000000000000000, 0.000000000000000000, 1.000000000000000000 ) ) ;
#22355 = CARTESIAN_POINT ( 'NONE',  ( 3.849727973822421485E-15, 1.499999999999994449, 0.000000000000000000 ) ) ;
#22356 = DIRECTION ( 'NONE',  ( -0.4166911066143264564, 0.000000000000000000, -0.9090481404571091328 ) ) ;
#22357 = EDGE_LOOP ( 'NONE', ( #9825, #19489, #4607, #8432 ) ) ;
#22358 = AXIS2_PLACEMENT_3D ( 'NONE', #9909, #16793, #1197 ) ;
#22359 = DIRECTION ( 'NONE',  ( 6.505213034913038160E-19, 3.903127820947822896E-18, 1.000000000000000000 ) ) ;
#22360 = DIRECTION ( 'NONE',  ( 0.000000000000000000, 1.000000000000000000, 0.000000000000000000 ) ) ;
#22361 = CARTESIAN_POINT ( 'NONE',  ( 1.072795092646390724, 5.000000000000002665, 38.73397172404480671 ) ) ;
#22362 = EDGE_CURVE ( 'NONE', #17743, #18756, #15638, .T. ) ;
#22363 = EDGE_CURVE ( 'NONE', #8737, #8568, #7991, .T. ) ;
#22364 = EDGE_CURVE ( 'NONE', #3496, #14915, #6557, .T. ) ;
#22365 = VERTEX_POINT ( 'NONE', #3113 ) ;
#22366 = EDGE_CURVE ( 'NONE', #11842, #1931, #15294, .T. ) ;
#22367 = CONTEXT_DEPENDENT_SHAPE_REPRESENTATION ( #1704, #22131 ) ;
#22368 = ORIENTED_EDGE ( 'NONE', *, *, #14617, .T. ) ;
#22369 = CARTESIAN_POINT ( 'NONE',  ( 34.99999999999980815, 40.00000000000000711, 54.99999999999922551 ) ) ;
#22370 = DIRECTION ( 'NONE',  ( -1.000000000000000000, 0.000000000000000000, 0.000000000000000000 ) ) ;
#22371 = CIRCLE ( 'NONE', #12461, 50.00000000000000000 ) ;
#22372 = FACE_OUTER_BOUND ( 'NONE', #264, .T. ) ;
#22373 = CARTESIAN_POINT ( 'NONE',  ( 18.11182660255252230, 11.48022137427003564, 60.14030069439205306 ) ) ;
#22374 = DIRECTION ( 'NONE',  ( -0.000000000000000000, -1.000000000000000000, -0.000000000000000000 ) ) ;
#22375 = ORIENTED_EDGE ( 'NONE', *, *, #7749, .T. ) ;
#22376 = CARTESIAN_POINT ( 'NONE',  ( -23.74488952252773544, 25.58633464742632313, 3.000000000000023537 ) ) ;
#22377 = DIRECTION ( 'NONE',  ( -0.000000000000000000, -0.000000000000000000, -1.000000000000000000 ) ) ;
#22378 = ORIENTED_EDGE ( 'NONE', *, *, #3068, .T. ) ;
#22379 = CARTESIAN_POINT ( 'NONE',  ( -11.86180952234344588, 38.99999999999292299, 55.35904751185378103 ) ) ;
#22380 = CARTESIAN_POINT ( 'NONE',  ( -35.00000000000000000, 38.99999999999999289, -59.99999999999998579 ) ) ;
#22381 = LINE ( 'NONE', #6670, #2379 ) ;
#22382 = DIRECTION ( 'NONE',  ( 6.505213034913038160E-19, 3.903127820947822896E-18, 1.000000000000000000 ) ) ;
#22383 = VERTEX_POINT ( 'NONE', #1276 ) ;
#22384 = CARTESIAN_POINT ( 'NONE',  ( -8.118562887736894496, 39.55762400984859539, -53.90122742181765858 ) ) ;
#22385 = EDGE_LOOP ( 'NONE', ( #11832, #6407 ) ) ;
#22386 = CARTESIAN_POINT ( 'NONE',  ( -32.83234229683721850, 11.85401191286866762, -2.999999999999971578 ) ) ;
#22387 = CARTESIAN_POINT ( 'NONE',  ( -13.56354382738803466, 2.142135623730931471, 56.03997097393687454 ) ) ;
#22388 = ORIENTED_EDGE ( 'NONE', *, *, #22363, .F. ) ;
#22389 = DIRECTION ( 'NONE',  ( 1.000000000000000000, 0.000000000000000000, 0.000000000000000000 ) ) ;
#22390 = CARTESIAN_POINT ( 'NONE',  ( 35.00000000000000711, 40.00000000000000000, 60.00000000000000711 ) ) ;
#22391 = DIRECTION ( 'NONE',  ( -6.505213034913038160E-19, -3.903127820947822896E-18, -1.000000000000000000 ) ) ;
#22392 = CARTESIAN_POINT ( 'NONE',  ( 19.88294660283887794, 17.66261523022804880, -60.59423886784173163 ) ) ;
#22394 = EDGE_CURVE ( 'NONE', #14544, #3949, #18924, .T. ) ;
#22393 = ORIENTED_EDGE ( 'NONE', *, *, #7647, .T. ) ;
#22395 = EDGE_CURVE ( 'NONE', #15748, #22593, #1049, .T. ) ;
#22396 = ORIENTED_EDGE ( 'NONE', *, *, #4435, .F. ) ;
#22397 = VERTEX_POINT ( 'NONE', #19153 ) ;
#22398 = VERTEX_POINT ( 'NONE', #1735 ) ;
#22399 = CARTESIAN_POINT ( 'NONE',  ( 6.696867368503558448E-15, 39.00000000000000711, 48.73397172404481381 ) ) ;
#22400 = CARTESIAN_POINT ( 'NONE',  ( 11.35354668330712613, 30.33632613426179248, -6.999999999999985789 ) ) ;
#22401 = AXIS2_PLACEMENT_3D ( 'NONE', #22369, #10079, #17074 ) ;
#22402 = LINE ( 'NONE', #8632, #15009 ) ;
#22403 = EDGE_CURVE ( 'NONE', #14085, #6835, #1416, .T. ) ;
#22404 = EDGE_LOOP ( 'NONE', ( #313, #10077, #19999, #15503 ) ) ;
#22405 = DIRECTION ( 'NONE',  ( 0.000000000000000000, 1.000000000000000000, 0.000000000000000000 ) ) ;
#22406 = LINE ( 'NONE', #16667, #770 ) ;
#22407 = EDGE_LOOP ( 'NONE', ( #7345, #14385, #18919, #10568 ) ) ;
#22408 = DIRECTION ( 'NONE',  ( 1.296372316667914327E-16, 1.000000000000000000, -0.000000000000000000 ) ) ;
#22409 = DIRECTION ( 'NONE',  ( 6.505213034913038160E-19, 3.903127820947822896E-18, 1.000000000000000000 ) ) ;
#22410 = CARTESIAN_POINT ( 'NONE',  ( 34.11307262910447236, -11.98990878915382119, -2.932164912090505560 ) ) ;
#22411 = CARTESIAN_POINT ( 'NONE',  ( 0.000000000000000000, 30.00000000000000000, 0.000000000000000000 ) ) ;
#22412 = CARTESIAN_POINT ( 'NONE',  ( -1.952222864267822100, 39.97720380408218688, 50.19196443857154577 ) ) ;
#22413 = CARTESIAN_POINT ( 'NONE',  ( 0.000000000000000000, -40.00000000000000000, 0.000000000000000000 ) ) ;
#22414 = ADVANCED_FACE ( 'NONE', ( #8720, #10084 ), #15579, .T. ) ;
#22415 = CIRCLE ( 'NONE', #11422, 2.499999999999995115 ) ;
#22416 = CARTESIAN_POINT ( 'NONE',  ( -14.69988787053504709, 16.91499873015103006, 45.69379240540681053 ) ) ;
#22417 = ORIENTED_EDGE ( 'NONE', *, *, #18946, .F. ) ;
#22418 = EDGE_LOOP ( 'NONE', ( #9573, #21988 ) ) ;
#22419 = VERTEX_POINT ( 'NONE', #13740 ) ;
#22420 = ORIENTED_EDGE ( 'NONE', *, *, #9001, .F. ) ;
#22421 = DIRECTION ( 'NONE',  ( -1.000000000000000000, -1.208970125616077665E-17, 0.000000000000000000 ) ) ;
#22422 = CARTESIAN_POINT ( 'NONE',  ( -11.99999999999985434, -1.500000000000013767, 0.000000000000000000 ) ) ;
#22423 = FACE_OUTER_BOUND ( 'NONE', #1840, .T. ) ;
#22424 = DIRECTION ( 'NONE',  ( -0.1421319796954322034, 0.000000000000000000, 0.9898477157360405787 ) ) ;
#22425 = CARTESIAN_POINT ( 'NONE',  ( -12.24744603030441148, 40.00000000000000000, 54.43639671998950291 ) ) ;
#22426 = VECTOR ( 'NONE', #21403, 1000.000000000000000 ) ;
#22427 = AXIS2_PLACEMENT_3D ( 'NONE', #3292, #1797, #17592 ) ;
#22428 = ORIENTED_EDGE ( 'NONE', *, *, #8209, .F. ) ;
#22429 = DIRECTION ( 'NONE',  ( 0.000000000000000000, -1.000000000000000000, 0.000000000000000000 ) ) ;
#22430 = CARTESIAN_POINT ( 'NONE',  ( -7.248955618538786894, 40.00000000000000711, -52.65401628672144341 ) ) ;
#22431 = CARTESIAN_POINT ( 'NONE',  ( 35.00000000000000711, 38.99999999999999289, 60.00000000000000711 ) ) ;
#22432 = DIRECTION ( 'NONE',  ( 0.000000000000000000, 0.000000000000000000, -1.000000000000000000 ) ) ;
#22433 = EDGE_CURVE ( 'NONE', #15811, #5732, #20980, .T. ) ;
#22434 = ORIENTED_EDGE ( 'NONE', *, *, #1598, .F. ) ;
#22435 = DIRECTION ( 'NONE',  ( -1.000000000000000000, -1.208970125616077665E-17, 0.000000000000000000 ) ) ;
#22436 = CARTESIAN_POINT ( 'NONE',  ( -10.77132920892044154, 39.17511451495860797, 54.93228420925925093 ) ) ;
#22437 = EDGE_CURVE ( 'NONE', #12610, #8443, #6918, .T. ) ;
#22438 = ORIENTED_EDGE ( 'NONE', *, *, #9510, .T. ) ;
#22439 = CARTESIAN_POINT ( 'NONE',  ( -4.080045426412826082, 32.20238537491803754, -2.999999999999971578 ) ) ;
#22440 = EDGE_CURVE ( 'NONE', #4768, #13346, #1619, .T. ) ;
#22441 = DIRECTION ( 'NONE',  ( -1.000000000000000000, -1.208970125616081209E-17, 0.000000000000000000 ) ) ;
#22442 = DIRECTION ( 'NONE',  ( -0.000000000000000000, 1.000000000000000000, -0.000000000000000000 ) ) ;
#22443 = DIRECTION ( 'NONE',  ( 6.505213034913038160E-19, 3.903127820947822896E-18, 1.000000000000000000 ) ) ;
#22444 = ORIENTED_EDGE ( 'NONE', *, *, #19406, .F. ) ;
#22445 = AXIS2_PLACEMENT_3D ( 'NONE', #17760, #17986, #2066 ) ;
#22446 = VECTOR ( 'NONE', #8782, 1000.000000000000000 ) ;
#22447 = AXIS2_PLACEMENT_3D ( 'NONE', #3925, #21567, #9416 ) ;
#22448 = ORIENTED_EDGE ( 'NONE', *, *, #15228, .F. ) ;
#22449 = CARTESIAN_POINT ( 'NONE',  ( -1.533556059876706179, -4.618461881322652118, 46.62226723458652344 ) ) ;
#22450 = EDGE_CURVE ( 'NONE', #454, #4439, #21172, .T. ) ;
#22451 = DIRECTION ( 'NONE',  ( -0.000000000000000000, 1.000000000000000000, -0.000000000000000000 ) ) ;
#22452 = ORIENTED_EDGE ( 'NONE', *, *, #12614, .T. ) ;
#22453 = DIRECTION ( 'NONE',  ( 0.000000000000000000, -1.000000000000000000, 0.000000000000000000 ) ) ;
#22454 = CIRCLE ( 'NONE', #12549, 9.000000000000035527 ) ;
#22455 = LINE ( 'NONE', #17274, #18391 ) ;
#22456 = CARTESIAN_POINT ( 'NONE',  ( -22.26748298433256679, 22.28024240313483517, 2.999999999999995559 ) ) ;
#22457 = ADVANCED_FACE ( 'NONE', ( #12046 ), #11808, .F. ) ;
#22458 = CARTESIAN_POINT ( 'NONE',  ( -18.96886095803721517, 26.35434275172291407, -60.36758075326453366 ) ) ;
#22459 = CARTESIAN_POINT ( 'NONE',  ( -42.50000000000000711, -5.000000000000000000, -47.50000000000000000 ) ) ;
#22460 = CARTESIAN_POINT ( 'NONE',  ( -15.90155957501130146, 35.87083899979363366, 56.88316157031724174 ) ) ;
#22461 = ORIENTED_EDGE ( 'NONE', *, *, #8073, .F. ) ;
#22462 = CARTESIAN_POINT ( 'NONE',  ( 5.833333333333338366, 33.81926995981415729, 40.61164310337067462 ) ) ;
#22463 = SURFACE_STYLE_USAGE ( .BOTH. , #5268 ) ;
#22464 = AXIS2_PLACEMENT_3D ( 'NONE', #13723, #15338, #1257 ) ;
#22465 = B_SPLINE_CURVE_WITH_KNOTS ( 'NONE', 3,
 ( #12697, #7780, #14752, #16132 ),
 .UNSPECIFIED., .F., .F.,
 ( 4, 4 ),
 ( 0.001875451646902692423, 0.003761979286331381712 ),
 .UNSPECIFIED. ) ;
#22466 = DIRECTION ( 'NONE',  ( 1.000000000000000000, 2.269002777743560714E-17, 0.000000000000000000 ) ) ;
#22467 = DIRECTION ( 'NONE',  ( 0.000000000000000000, 0.000000000000000000, -1.000000000000000000 ) ) ;
#22468 = CIRCLE ( 'NONE', #11474, 8.999999999999998224 ) ;
#22469 = EDGE_CURVE ( 'NONE', #12370, #19815, #14183, .T. ) ;
#22470 = VERTEX_POINT ( 'NONE', #10201 ) ;
#22471 = CARTESIAN_POINT ( 'NONE',  ( 35.00000000000001421, -5.000000000000000000, 1.540743955509788682E-30 ) ) ;
#22472 = CARTESIAN_POINT ( 'NONE',  ( -34.99999999999999289, 39.00000000000000711, -49.99999999999997158 ) ) ;
#22473 = CONICAL_SURFACE ( 'NONE', #10728, 17.00000000000001421, 0.7853981633974603804 ) ;
#22474 = EDGE_LOOP ( 'NONE', ( #17453, #16074, #4666, #16110 ) ) ;
#22475 = AXIS2_PLACEMENT_3D ( 'NONE', #21515, #16348, #658 ) ;
#22476 = EDGE_CURVE ( 'NONE', #5574, #5004, #16792, .T. ) ;
#22477 = DIRECTION ( 'NONE',  ( 0.000000000000000000, 0.000000000000000000, 1.000000000000000000 ) ) ;
#22478 = AXIS2_PLACEMENT_3D ( 'NONE', #5512, #14664, #7234 ) ;
#22479 = ORIENTED_EDGE ( 'NONE', *, *, #11783, .T. ) ;
#22480 = CARTESIAN_POINT ( 'NONE',  ( 26.50842683089768670, -24.41514043009201984, 2.999999999999995559 ) ) ;
#22481 = DIRECTION ( 'NONE',  ( -6.505213034913038160E-19, -3.903127820947822896E-18, -1.000000000000000000 ) ) ;
#22482 = FACE_OUTER_BOUND ( 'NONE', #13982, .T. ) ;
#22483 = CYLINDRICAL_SURFACE ( 'NONE', #7968, 22.00000000000000000 ) ;
#22484 = DIRECTION ( 'NONE',  ( -1.000000000000000000, 0.000000000000000000, 0.000000000000000000 ) ) ;
#22485 = ORIENTED_EDGE ( 'NONE', *, *, #3026, .T. ) ;
#22486 = DIRECTION ( 'NONE',  ( 6.505213034913038160E-19, 3.903127820947822896E-18, 1.000000000000000000 ) ) ;
#22487 = CARTESIAN_POINT ( 'NONE',  ( 9.708269511265326557, -33.52953626616050542, 3.000000000000002665 ) ) ;
#22488 = ORIENTED_EDGE ( 'NONE', *, *, #893, .F. ) ;
#22489 = EDGE_CURVE ( 'NONE', #15378, #3909, #6662, .T. ) ;
#22490 = CARTESIAN_POINT ( 'NONE',  ( -6.000000000000000000, -20.00000000000000000, -5.999999999999999112 ) ) ;
#22491 = FACE_OUTER_BOUND ( 'NONE', #19726, .T. ) ;
#22492 = CARTESIAN_POINT ( 'NONE',  ( 8.555717054908910768, 39.50215801961479656, 54.09939909776313272 ) ) ;
#22493 = ORIENTED_EDGE ( 'NONE', *, *, #2125, .T. ) ;
#22494 = CARTESIAN_POINT ( 'NONE',  ( -5.400043222043034774, 39.81718168819095638, -52.45350590964093840 ) ) ;
#22495 = ORIENTED_EDGE ( 'NONE', *, *, #6337, .F. ) ;
#22496 = DIRECTION ( 'NONE',  ( -6.505213034913038160E-19, -3.903127820947822896E-18, -1.000000000000000000 ) ) ;
#22497 = CARTESIAN_POINT ( 'NONE',  ( -22.34927643452058632, 22.00360349561975326, 58.65118246389018708 ) ) ;
#22498 = VERTEX_POINT ( 'NONE', #20874 ) ;
#22499 = CYLINDRICAL_SURFACE ( 'NONE', #8692, 1.000000000000000888 ) ;
#22500 = CARTESIAN_POINT ( 'NONE',  ( -12.00937115242646591, -34.74700806321101254, 2.800654218530512551 ) ) ;
#22501 = EDGE_CURVE ( 'NONE', #22194, #13976, #16967, .T. ) ;
#22502 = DIRECTION ( 'NONE',  ( -0.000000000000000000, -1.000000000000000000, -0.000000000000000000 ) ) ;
#22503 = VECTOR ( 'NONE', #3671, 1000.000000000000000 ) ;
#22504 = CARTESIAN_POINT ( 'NONE',  ( 11.68090480754628402, 3.765577839755378076, -57.90797000640140624 ) ) ;
#22505 = EDGE_CURVE ( 'NONE', #9422, #16292, #13474, .T. ) ;
#22506 = VERTEX_POINT ( 'NONE', #15799 ) ;
#22507 = EDGE_LOOP ( 'NONE', ( #16199, #2997, #7187, #18582 ) ) ;
#22508 = EDGE_CURVE ( 'NONE', #19216, #19994, #4350, .T. ) ;
#22509 = CONICAL_SURFACE ( 'NONE', #16272, 8.999999999999973355, 0.7853981633974657095 ) ;
#22510 = VERTEX_POINT ( 'NONE', #3572 ) ;
#22511 = FACE_OUTER_BOUND ( 'NONE', #6120, .T. ) ;
#22512 = ORIENTED_EDGE ( 'NONE', *, *, #15091, .T. ) ;
#22513 = CARTESIAN_POINT ( 'NONE',  ( -27.56232195404058416, 21.41958700883256483, -2.999999999999971578 ) ) ;
#22514 = CIRCLE ( 'NONE', #21768, 6.499999999999999112 ) ;
#22515 = CARTESIAN_POINT ( 'NONE',  ( 11.86180952233169705, 39.00000000000000000, 55.35904751184887118 ) ) ;
#22516 = CARTESIAN_POINT ( 'NONE',  ( 6.488138469136647934, 39.99999999999999289, -52.32258420267954335 ) ) ;
#22517 = EDGE_LOOP ( 'NONE', ( #5608, #5203, #12496, #3655 ) ) ;
#22518 = FACE_OUTER_BOUND ( 'NONE', #5603, .T. ) ;
#22519 = LINE ( 'NONE', #5107, #19313 ) ;
#22520 = ORIENTED_EDGE ( 'NONE', *, *, #4252, .F. ) ;
#22521 = CARTESIAN_POINT ( 'NONE',  ( -5.510194049583325260, 0.6966826613253894740, 52.42111735158517405 ) ) ;
#22522 = EDGE_CURVE ( 'NONE', #14603, #5777, #14302, .T. ) ;
#22523 = CARTESIAN_POINT ( 'NONE',  ( 4.986731981817641213, 34.15484146257775677, 40.05110651909060238 ) ) ;
#22524 = ORIENTED_EDGE ( 'NONE', *, *, #6949, .F. ) ;
#22525 = CARTESIAN_POINT ( 'NONE',  ( 7.938322399564428089, 38.36220367130324860, -56.16250688144687331 ) ) ;
#22526 = CARTESIAN_POINT ( 'NONE',  ( -34.99999999999999289, -3.999999999999985345, 59.99999999999698019 ) ) ;
#22527 = AXIS2_PLACEMENT_3D ( 'NONE', #4685, #18540, #6283 ) ;
#22528 = CARTESIAN_POINT ( 'NONE',  ( 29.32895111104242503, 20.05817253550603851, -2.999999999999993339 ) ) ;
#22529 = DIRECTION ( 'NONE',  ( 1.000000000000000000, 0.000000000000000000, 0.000000000000000000 ) ) ;
#22530 = ADVANCED_FACE ( 'NONE', ( #10874 ), #5607, .F. ) ;
#22531 = EDGE_CURVE ( 'NONE', #9680, #10638, #12393, .T. ) ;
#22532 = DIRECTION ( 'NONE',  ( -6.505213034913038160E-19, -3.903127820947822896E-18, -1.000000000000000000 ) ) ;
#22533 = CIRCLE ( 'NONE', #9356, 0.9999999999999974465 ) ;
#22534 = CARTESIAN_POINT ( 'NONE',  ( -42.49999999999996447, 10.00000000000000000, -47.50000000000000711 ) ) ;
#22535 = EDGE_CURVE ( 'NONE', #16319, #22498, #16261, .T. ) ;
#22536 = VERTEX_POINT ( 'NONE', #10637 ) ;
#22537 = VERTEX_POINT ( 'NONE', #10752 ) ;
#22538 = ORIENTED_EDGE ( 'NONE', *, *, #6446, .T. ) ;
#22539 = CIRCLE ( 'NONE', #1675, 11.00000000000003730 ) ;
#22540 = ORIENTED_EDGE ( 'NONE', *, *, #19694, .T. ) ;
#22541 = DIRECTION ( 'NONE',  ( 6.505213034913038160E-19, 3.903127820947822896E-18, 1.000000000000000000 ) ) ;
#22542 = DIRECTION ( 'NONE',  ( -1.000000000000000000, -1.208970125616046080E-17, 6.505213034913038160E-19 ) ) ;
#22543 = CIRCLE ( 'NONE', #6430, 31.50000000000000711 ) ;
#22544 = DIRECTION ( 'NONE',  ( 1.049727191138617217E-16, 0.5150380749100562650, -0.8571673007021111124 ) ) ;
#22545 = VECTOR ( 'NONE', #16476, 1000.000000000000000 ) ;
#22546 = CARTESIAN_POINT ( 'NONE',  ( 4.589694779437865968, 39.86882943453918671, 51.95767925715862390 ) ) ;
#22547 = VECTOR ( 'NONE', #13812, 1000.000000000000000 ) ;
#22548 = EDGE_LOOP ( 'NONE', ( #11221, #11095 ) ) ;
#22549 = DIRECTION ( 'NONE',  ( 0.000000000000000000, -0.000000000000000000, -1.000000000000000000 ) ) ;
#22550 = DIRECTION ( 'NONE',  ( -1.000000000000000000, 0.000000000000000000, 0.000000000000000000 ) ) ;
#22551 = CARTESIAN_POINT ( 'NONE',  ( -34.90673715956756240, -1.391773526489529182E-13, 2.999999999999999112 ) ) ;
#22552 = CARTESIAN_POINT ( 'NONE',  ( 9.952189117650780403, 40.00000000000000000, -53.64426396172070355 ) ) ;
#22553 = CARTESIAN_POINT ( 'NONE',  ( 3.469446951953614189E-15, 38.23275711891355400, 0.000000000000000000 ) ) ;
#22554 = EDGE_CURVE ( 'NONE', #13097, #15034, #21550, .T. ) ;
#22555 = ORIENTED_EDGE ( 'NONE', *, *, #11553, .F. ) ;
#22556 = FACE_OUTER_BOUND ( 'NONE', #12242, .T. ) ;
#22557 = CARTESIAN_POINT ( 'NONE',  ( -17.90966157241563650, 28.91510314404815318, 60.08313820791177307 ) ) ;
#22558 = VECTOR ( 'NONE', #8495, 1000.000000000000000 ) ;
#22559 = CONICAL_SURFACE ( 'NONE', #12281, 2.099999999999990763, 1.029744258676652091 ) ;
#22560 = EDGE_LOOP ( 'NONE', ( #18155, #16076, #13003, #20312 ) ) ;
#22561 = DIRECTION ( 'NONE',  ( 1.000000000000000000, 0.000000000000000000, 0.000000000000000000 ) ) ;
#22562 = CARTESIAN_POINT ( 'NONE',  ( 1.387778780781445676E-14, 0.000000000000000000, -1.506085580481783063E-14 ) ) ;
#22563 = ADVANCED_FACE ( 'NONE', ( #9056 ), #9838, .F. ) ;
#22564 = FACE_BOUND ( 'NONE', #2471, .T. ) ;
#22565 = CARTESIAN_POINT ( 'NONE',  ( 4.000000000000003553, 1.499999999999996447, 0.000000000000000000 ) ) ;
#22566 = EDGE_LOOP ( 'NONE', ( #15455, #741, #12834, #7517 ) ) ;
#22567 = CIRCLE ( 'NONE', #17780, 34.90673715956759082 ) ;
#22568 = ADVANCED_FACE ( 'NONE', ( #4031 ), #3908, .F. ) ;
#22569 = ORIENTED_EDGE ( 'NONE', *, *, #2211, .F. ) ;
#22570 = CARTESIAN_POINT ( 'NONE',  ( 4.026578693505867612, -4.679980696183926980, -48.24134193084080380 ) ) ;
#22571 = CARTESIAN_POINT ( 'NONE',  ( -17.32050807568833051, 1.500000000000015099, -10.00000000000047251 ) ) ;
#22572 = AXIS2_PLACEMENT_3D ( 'NONE', #5076, #6564, #1398 ) ;
#22573 = AXIS2_PLACEMENT_3D ( 'NONE', #22207, #19101, #15412 ) ;
#22574 = AXIS2_PLACEMENT_3D ( 'NONE', #8837, #13870, #10431 ) ;
#22575 = ORIENTED_EDGE ( 'NONE', *, *, #15313, .T. ) ;
#22576 = ADVANCED_FACE ( 'NONE', ( #450 ), #2288, .F. ) ;
#22577 = CARTESIAN_POINT ( 'NONE',  ( -34.99999999999999289, -5.000000000000000000, -54.99999999999705125 ) ) ;
#22578 = DIRECTION ( 'NONE',  ( 0.000000000000000000, 0.000000000000000000, 1.000000000000000000 ) ) ;
#22579 = CARTESIAN_POINT ( 'NONE',  ( 10.39230484541308819, 1.500000000000004885, 6.000000000000008882 ) ) ;
#22580 = CARTESIAN_POINT ( 'NONE',  ( -19.23106185100149901, 25.51013774189691929, -60.43438466297349976 ) ) ;
#22581 = DIRECTION ( 'NONE',  ( 0.000000000000000000, -0.5150380749100547106, -0.8571673007021120005 ) ) ;
#22582 = AXIS2_PLACEMENT_3D ( 'NONE', #19792, #7643, #649 ) ;
#22583 = VERTEX_POINT ( 'NONE', #12584 ) ;
#22584 = DIRECTION ( 'NONE',  ( 0.000000000000000000, 1.000000000000000000, 0.000000000000000000 ) ) ;
#22585 = DIRECTION ( 'NONE',  ( -1.000000000000000000, 0.000000000000000000, 0.000000000000000000 ) ) ;
#22586 = CARTESIAN_POINT ( 'NONE',  ( -34.99999999999980815, 26.00000000000000355, 54.99999999999922551 ) ) ;
#22587 = FACE_OUTER_BOUND ( 'NONE', #9934, .T. ) ;
#22588 = ORIENTED_EDGE ( 'NONE', *, *, #3879, .T. ) ;
#22589 = LINE ( 'NONE', #17746, #6432 ) ;
#22590 = DIRECTION ( 'NONE',  ( 1.000000000000000000, 0.000000000000000000, 0.000000000000000000 ) ) ;
#22591 = VECTOR ( 'NONE', #11009, 1000.000000000000000 ) ;
#22592 = EDGE_CURVE ( 'NONE', #17930, #11125, #9365, .T. ) ;
#22593 = VERTEX_POINT ( 'NONE', #19383 ) ;
#22594 = AXIS2_PLACEMENT_3D ( 'NONE', #13073, #16761, #9772 ) ;
#22595 = APPLICATION_PROTOCOL_DEFINITION ( 'draft international standard', 'automotive_design', 1998, #16917 ) ;
#22596 = ORIENTED_EDGE ( 'NONE', *, *, #13250, .F. ) ;
#22597 = LINE ( 'NONE', #6894, #14296 ) ;
#22598 = EDGE_CURVE ( 'NONE', #9329, #4860, #17132, .T. ) ;
#22599 = CARTESIAN_POINT ( 'NONE',  ( -0.05567163768954545844, -4.650449146058876160, 45.38800358221619291 ) ) ;
#22600 = DIRECTION ( 'NONE',  ( -6.505213034913038160E-19, -3.903127820947822896E-18, -1.000000000000000000 ) ) ;
#22601 = DIRECTION ( 'NONE',  ( 0.000000000000000000, 0.000000000000000000, 1.000000000000000000 ) ) ;
#22602 = DIRECTION ( 'NONE',  ( -0.000000000000000000, -0.000000000000000000, 1.000000000000000000 ) ) ;
#22603 = VECTOR ( 'NONE', #16871, 1000.000000000000000 ) ;
#22604 = EDGE_LOOP ( 'NONE', ( #1530, #6156, #8395, #2151, #7627 ) ) ;
#22605 = DIRECTION ( 'NONE',  ( -1.000000000000000000, -1.208970125616060101E-17, 6.505213034913038160E-19 ) ) ;
#22606 = LINE ( 'NONE', #5181, #7216 ) ;
#22607 = ORIENTED_EDGE ( 'NONE', *, *, #19940, .T. ) ;
#22608 = DIRECTION ( 'NONE',  ( -6.505213034913038160E-19, -3.903127820947822896E-18, -1.000000000000000000 ) ) ;
#22609 = AXIS2_PLACEMENT_3D ( 'NONE', #12904, #16584, #19810 ) ;
#22610 = DIRECTION ( 'NONE',  ( 0.000000000000000000, 1.000000000000000000, 0.000000000000000000 ) ) ;
#22611 = CARTESIAN_POINT ( 'NONE',  ( 6.696867368503558448E-15, 40.00000000000000000, 38.73397172404480671 ) ) ;
#22612 = CARTESIAN_POINT ( 'NONE',  ( 7.902600813477331343, 39.58333018208552545, 53.79900148939188398 ) ) ;
#22613 = CARTESIAN_POINT ( 'NONE',  ( 14.99999999999998934, 20.38555233723673155, -45.82575694955836809 ) ) ;
#22614 = VERTEX_POINT ( 'NONE', #16137 ) ;
#22615 = DIRECTION ( 'NONE',  ( -1.000000000000000000, -1.208970125616081209E-17, 0.000000000000000000 ) ) ;
#22616 = CARTESIAN_POINT ( 'NONE',  ( -22.27968669415840708, 17.44229586407519506, 58.63614535158255592 ) ) ;
#22617 = ORIENTED_EDGE ( 'NONE', *, *, #8898, .T. ) ;
#22618 = DIRECTION ( 'NONE',  ( -0.000000000000000000, 1.000000000000000000, -0.000000000000000000 ) ) ;
#22619 = EDGE_CURVE ( 'NONE', #21644, #3949, #10922, .T. ) ;
#22620 = CIRCLE ( 'NONE', #6151, 2.524999999999999467 ) ;
#22621 = CIRCLE ( 'NONE', #16372, 57.07106781186551103 ) ;
#22622 = DIRECTION ( 'NONE',  ( -1.000000000000000000, 0.000000000000000000, 0.000000000000000000 ) ) ;
#22623 = CARTESIAN_POINT ( 'NONE',  ( 24.10368028608819913, -26.10969099697642193, -2.999999999999983125 ) ) ;
#22624 = AXIS2_PLACEMENT_3D ( 'NONE', #16171, #484, #7481 ) ;
#22625 = CARTESIAN_POINT ( 'NONE',  ( 42.50000000000000711, -9.600000000000001421, 47.50000000000000711 ) ) ;
#22626 = VECTOR ( 'NONE', #14986, 1000.000000000000000 ) ;
#22627 = EDGE_CURVE ( 'NONE', #1608, #675, #5848, .T. ) ;
#22628 = ADVANCED_FACE ( 'NONE', ( #17538 ), #2526, .T. ) ;
#22629 = EDGE_LOOP ( 'NONE', ( #4554, #21351 ) ) ;
#22630 = ORIENTED_EDGE ( 'NONE', *, *, #14322, .T. ) ;
#22631 = VERTEX_POINT ( 'NONE', #21203 ) ;
#22632 =( NAMED_UNIT ( * ) PLANE_ANGLE_UNIT ( ) SI_UNIT ( $, .RADIAN. ) );
#22633 = ORIENTED_EDGE ( 'NONE', *, *, #6883, .F. ) ;
#22634 = CARTESIAN_POINT ( 'NONE',  ( 4.456525674222657894E-15, 6.180736333215575584, 0.000000000000000000 ) ) ;
#22635 = DIRECTION ( 'NONE',  ( -6.505213034913038160E-19, -3.903127820947822896E-18, -1.000000000000000000 ) ) ;
#22636 = CYLINDRICAL_SURFACE ( 'NONE', #9173, 2.099999999999997868 ) ;
#22637 = CARTESIAN_POINT ( 'NONE',  ( 0.9873823069974712041, 39.99999999999999289, 49.36449633666812531 ) ) ;
#22638 = AXIS2_PLACEMENT_3D ( 'NONE', #18290, #7746, #20016 ) ;
#22639 = ORIENTED_EDGE ( 'NONE', *, *, #4793, .F. ) ;
#22640 = CARTESIAN_POINT ( 'NONE',  ( -20.05817253550612023, 29.32895111104205199, -3.000000000000006661 ) ) ;
#22641 = CARTESIAN_POINT ( 'NONE',  ( 35.00000000000058265, 28.00000000000000000, -55.00000000000076028 ) ) ;
#22642 = VERTEX_POINT ( 'NONE', #19725 ) ;
#22643 = AXIS2_PLACEMENT_3D ( 'NONE', #2321, #9431, #14221 ) ;
#22644 = CIRCLE ( 'NONE', #2129, 2.099999999999997868 ) ;
#22645 = ORIENTED_EDGE ( 'NONE', *, *, #21648, .T. ) ;
#22646 = CYLINDRICAL_SURFACE ( 'NONE', #21911, 31.50000000000001421 ) ;
#22647 = VERTEX_POINT ( 'NONE', #14539 ) ;
#22648 = CARTESIAN_POINT ( 'NONE',  ( 8.234900601806485199, 38.24530923897635404, -54.56726664451450404 ) ) ;
#22649 = CIRCLE ( 'NONE', #5414, 2.000000000000000000 ) ;
#22650 = ADVANCED_FACE ( 'NONE', ( #12815 ), #7677, .F. ) ;
#22651 = CARTESIAN_POINT ( 'NONE',  ( 7.776554266669417956E-15, -4.648749848372173865, -45.43309249825056639 ) ) ;
#22652 = VECTOR ( 'NONE', #10699, 1000.000000000000000 ) ;
#22653 = CARTESIAN_POINT ( 'NONE',  ( -1.109399418554577021, 39.99267480748693515, 49.57771599688018682 ) ) ;
#22654 = EDGE_CURVE ( 'NONE', #1985, #7, #15310, .T. ) ;
#22655 = LINE ( 'NONE', #11433, #4227 ) ;
#22656 = DIRECTION ( 'NONE',  ( -1.000000000000000000, 1.764267138144086878E-15, 0.000000000000000000 ) ) ;
#22657 = DIRECTION ( 'NONE',  ( -0.000000000000000000, -0.000000000000000000, 1.000000000000000000 ) ) ;
#22658 = EDGE_CURVE ( 'NONE', #15733, #14756, #18261, .T. ) ;
#22659 = EDGE_CURVE ( 'NONE', #22194, #11090, #19721, .T. ) ;
#22660 = VERTEX_POINT ( 'NONE', #4863 ) ;
#22661 = CIRCLE ( 'NONE', #8005, 18.42595423422130452 ) ;
#22662 = ORIENTED_EDGE ( 'NONE', *, *, #20660, .F. ) ;
#22663 = EDGE_LOOP ( 'NONE', ( #12949, #1585 ) ) ;
#22664 = AXIS2_PLACEMENT_3D ( 'NONE', #6898, #17078, #13619 ) ;
#22665 = EDGE_CURVE ( 'NONE', #5947, #5980, #20786, .T. ) ;
#22666 = ORIENTED_EDGE ( 'NONE', *, *, #6028, .F. ) ;
#22667 = CYLINDRICAL_SURFACE ( 'NONE', #4104, 9.000000000000003553 ) ;
#22668 = DIRECTION ( 'NONE',  ( 0.000000000000000000, -1.000000000000000000, 0.000000000000000000 ) ) ;
#22669 = ADVANCED_FACE ( 'NONE', ( #13979, #22511 ), #1301, .T. ) ;
#22670 = DIRECTION ( 'NONE',  ( 6.505213034913038160E-19, 3.903127820947822896E-18, 1.000000000000000000 ) ) ;
#22671 = CARTESIAN_POINT ( 'NONE',  ( 0.1621097943337942160, 39.99984846037706632, 48.85976281227350881 ) ) ;
#22672 = ADVANCED_FACE ( 'NONE', ( #17331 ), #18954, .F. ) ;
#22673 = ORIENTED_EDGE ( 'NONE', *, *, #13247, .F. ) ;
#22674 = CARTESIAN_POINT ( 'NONE',  ( -34.99999999999999289, 5.000000000000000000, -3.012171160963566127E-14 ) ) ;
#22675 = DIRECTION ( 'NONE',  ( 1.000000000000000000, 0.000000000000000000, 0.000000000000000000 ) ) ;
#22676 = CARTESIAN_POINT ( 'NONE',  ( 2.775557561562891351E-14, -2.775557561562891351E-14, 2.999999999999999112 ) ) ;
#22677 = CARTESIAN_POINT ( 'NONE',  ( -1.387778780781445518E-14, 20.00000000000000355, -102.0000000000000142 ) ) ;
#22678 = DIRECTION ( 'NONE',  ( 0.000000000000000000, 1.000000000000000000, 0.000000000000000000 ) ) ;
#22679 = ORIENTED_EDGE ( 'NONE', *, *, #9439, .T. ) ;
#22680 = DIRECTION ( 'NONE',  ( 1.000000000000000000, 0.000000000000000000, 0.000000000000000000 ) ) ;
#22681 =( GEOMETRIC_REPRESENTATION_CONTEXT ( 3 ) GLOBAL_UNCERTAINTY_ASSIGNED_CONTEXT ( ( #960 ) ) GLOBAL_UNIT_ASSIGNED_CONTEXT ( ( #19624, #2204, #7472 ) ) REPRESENTATION_CONTEXT ( 'NONE', 'WORKASPACE' ) );
#22682 = CYLINDRICAL_SURFACE ( 'NONE', #17847, 1.000000000000000888 ) ;
#22683 = CARTESIAN_POINT ( 'NONE',  ( -20.17230487860793886, -25.34312177887360207, 2.999999999999995559 ) ) ;
#22684 = DIRECTION ( 'NONE',  ( 0.000000000000000000, 1.000000000000000000, 0.000000000000000000 ) ) ;
#22685 = DIRECTION ( 'NONE',  ( 6.505213034913038160E-19, 3.903127820947822896E-18, 1.000000000000000000 ) ) ;
#22686 = ORIENTED_EDGE ( 'NONE', *, *, #17581, .F. ) ;
#22687 = VERTEX_POINT ( 'NONE', #4973 ) ;
#22688 = EDGE_CURVE ( 'NONE', #4478, #1089, #8374, .T. ) ;
#22689 = ORIENTED_EDGE ( 'NONE', *, *, #10441, .T. ) ;
#22690 = FACE_OUTER_BOUND ( 'NONE', #6036, .T. ) ;
#22691 = EDGE_CURVE ( 'NONE', #11067, #5224, #5810, .T. ) ;
#22692 = CARTESIAN_POINT ( 'NONE',  ( 12.24744603030438839, 40.00000000000000000, -54.43639671998947449 ) ) ;
#22693 = ORIENTED_EDGE ( 'NONE', *, *, #10811, .T. ) ;
#22694 = FACE_OUTER_BOUND ( 'NONE', #9815, .T. ) ;
#22695 = EDGE_LOOP ( 'NONE', ( #9768, #7752, #22588, #21086 ) ) ;
#22696 = NEXT_ASSEMBLY_USAGE_OCCURRENCE ( 'NAUO1', ' ', ' ', #20341, #18657, $ ) ;
#22697 = NEXT_ASSEMBLY_USAGE_OCCURRENCE ( 'NAUO2', ' ', ' ', #20341, #17241, $ ) ;
#22698 = NEXT_ASSEMBLY_USAGE_OCCURRENCE ( 'NAUO3', ' ', ' ', #20341, #17947, $ ) ;
#22699 = NEXT_ASSEMBLY_USAGE_OCCURRENCE ( 'NAUO4', ' ', ' ', #20341, #22019, $ ) ;
#22700 = NEXT_ASSEMBLY_USAGE_OCCURRENCE ( 'NAUO5', ' ', ' ', #20341, #306, $ ) ;
#22701 = NEXT_ASSEMBLY_USAGE_OCCURRENCE ( 'NAUO6', ' ', ' ', #20341, #10506, $ ) ;
#22702 = NEXT_ASSEMBLY_USAGE_OCCURRENCE ( 'NAUO7', ' ', ' ', #20341, #7439, $ ) ;
#22703 = NEXT_ASSEMBLY_USAGE_OCCURRENCE ( 'NAUO8', ' ', ' ', #20341, #22019, $ ) ;
#22704 = NEXT_ASSEMBLY_USAGE_OCCURRENCE ( 'NAUO9', ' ', ' ', #20341, #306, $ ) ;
#22705 = NEXT_ASSEMBLY_USAGE_OCCURRENCE ( 'NAUO10', ' ', ' ', #20341, #18657, $ ) ;
#22706 = NEXT_ASSEMBLY_USAGE_OCCURRENCE ( 'NAUO11', ' ', ' ', #20341, #12887, $ ) ;
#22707=COLOUR_RGB('Dark Blue',0.08,0.2,0.34);
#22708=FILL_AREA_STYLE_COLOUR('',#22707);
#22709=FILL_AREA_STYLE('',(#22708));
#22710=SURFACE_STYLE_FILL_AREA(#22709);
#22711=SURFACE_SIDE_STYLE('',(#22710));
#22712=SURFACE_STYLE_USAGE(.BOTH.,#22711);
#22713=PRESENTATION_STYLE_ASSIGNMENT((#22712));
#22714=COLOUR_RGB('Light Blue',0.38,0.62,0.78);
#22715=FILL_AREA_STYLE_COLOUR('',#22714);
#22716=FILL_AREA_STYLE('',(#22715));
#22717=SURFACE_STYLE_FILL_AREA(#22716);
#22718=SURFACE_SIDE_STYLE('',(#22717));
#22719=SURFACE_STYLE_USAGE(.BOTH.,#22718);
#22720=PRESENTATION_STYLE_ASSIGNMENT((#22719));
#22721=COLOUR_RGB('Sky Blue',0.24,0.69,0.87);
#22722=FILL_AREA_STYLE_COLOUR('',#22721);
#22723=FILL_AREA_STYLE('',(#22722));
#22724=SURFACE_STYLE_FILL_AREA(#22723);
#22725=SURFACE_SIDE_STYLE('',(#22724));
#22726=SURFACE_STYLE_USAGE(.BOTH.,#22725);
#22727=PRESENTATION_STYLE_ASSIGNMENT((#22726));
#22728=COLOUR_RGB('Grey',0.48,0.52,0.57);
#22729=FILL_AREA_STYLE_COLOUR('',#22728);
#22730=FILL_AREA_STYLE('',(#22729));
#22731=SURFACE_STYLE_FILL_AREA(#22730);
#22732=SURFACE_SIDE_STYLE('',(#22731));
#22733=SURFACE_STYLE_USAGE(.BOTH.,#22732);
#22734=PRESENTATION_STYLE_ASSIGNMENT((#22733));
#22735=COLOUR_RGB('Black',0.12,0.14,0.17);
#22736=FILL_AREA_STYLE_COLOUR('',#22735);
#22737=FILL_AREA_STYLE('',(#22736));
#22738=SURFACE_STYLE_FILL_AREA(#22737);
#22739=SURFACE_SIDE_STYLE('',(#22738));
#22740=SURFACE_STYLE_USAGE(.BOTH.,#22739);
#22741=PRESENTATION_STYLE_ASSIGNMENT((#22740));
#22742=COLOUR_RGB('Off White',0.89,0.88,0.83);
#22743=FILL_AREA_STYLE_COLOUR('',#22742);
#22744=FILL_AREA_STYLE('',(#22743));
#22745=SURFACE_STYLE_FILL_AREA(#22744);
#22746=SURFACE_SIDE_STYLE('',(#22745));
#22747=SURFACE_STYLE_USAGE(.BOTH.,#22746);
#22748=PRESENTATION_STYLE_ASSIGNMENT((#22747));
ENDSEC;
END-ISO-10303-21;
